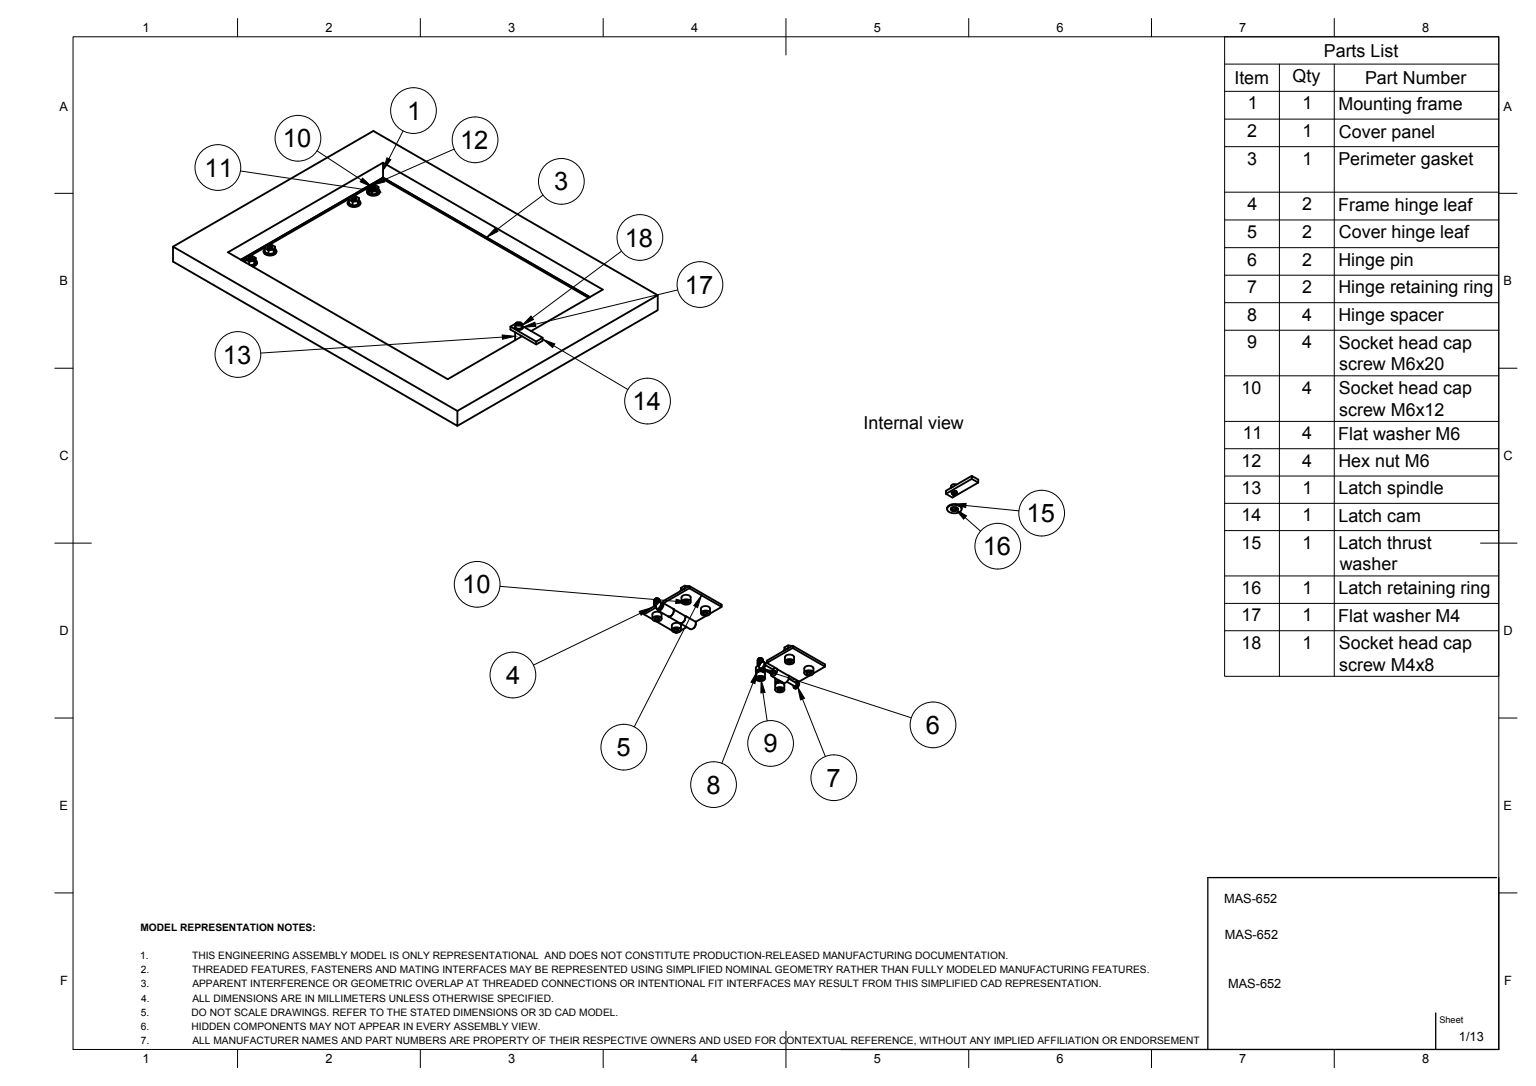
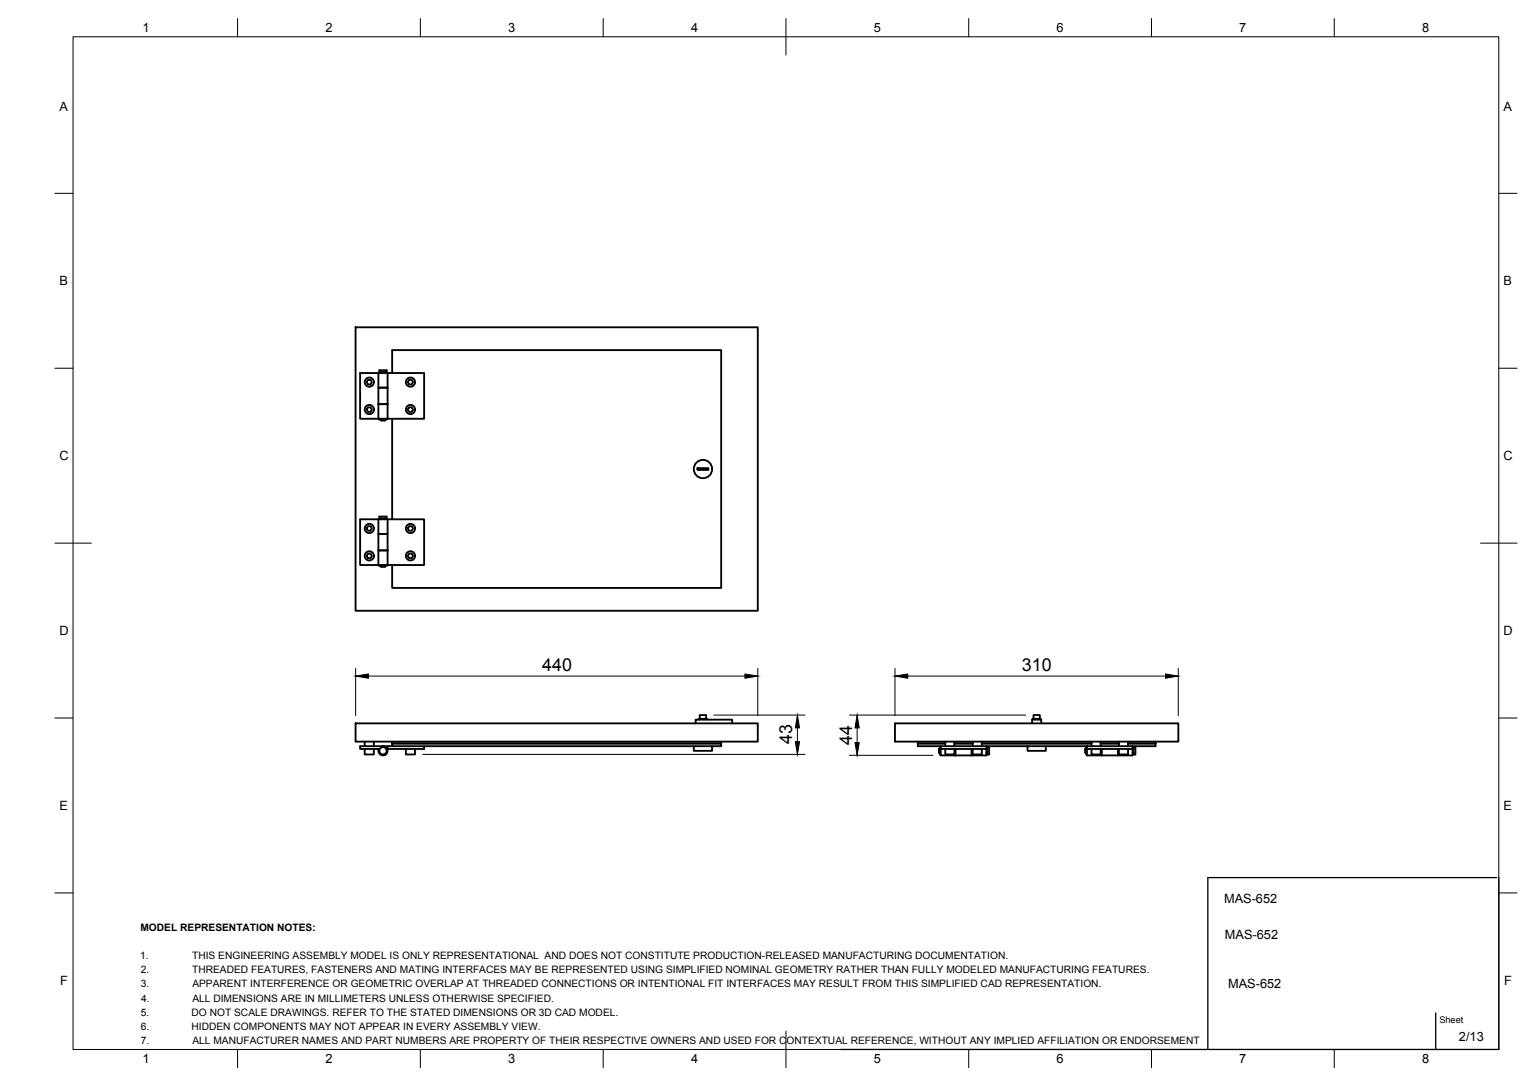
ISO-10303-21;
HEADER;
/* Generated by software containing ST-Developer
 * from STEP Tools, Inc. (www.steptools.com) 
 */

FILE_DESCRIPTION(
/* description */ ('Independent hinged machine back cover with retained hinge pins, perim
eter gasket and quarter-turn cam latch. Nominal cover 360 x 260 x 3 mm
, frame 430 x 300 x 20 mm. No guarding, structural or ingress rating a
ssigned.'),
/* implementation_level */ '2;1');

FILE_NAME(
/* name */ 'MAS-652.step',
/* time_stamp */ '2026-11-09T19:36:59-08:00',
/* author */ (''),
/* organization */ (''),
/* preprocessor_version */ 'ST-DEVELOPER v20.2',
/* originating_system */ 'Autodesk Translation Framework v15.17.0.0',
/* authorisation */ '');

FILE_SCHEMA (('AUTOMOTIVE_DESIGN { 1 0 10303 214 3 1 1 }'));
ENDSEC;

DATA;
#10=MECHANICAL_DESIGN_GEOMETRIC_PRESENTATION_REPRESENTATION('',(#198,#199,
#200,#201,#202,#203,#204,#205,#206,#207,#208,#209,#210,#211,#212,#213,#214,
#215),#32627);
#11=ITEM_DEFINED_TRANSFORMATION($,$,#8893,#9492);
#12=ITEM_DEFINED_TRANSFORMATION($,$,#9080,#9493);
#13=ITEM_DEFINED_TRANSFORMATION($,$,#9102,#9494);
#14=ITEM_DEFINED_TRANSFORMATION($,$,#9267,#9495);
#15=ITEM_DEFINED_TRANSFORMATION($,$,#9323,#9496);
#16=ITEM_DEFINED_TRANSFORMATION($,$,#9294,#9497);
#17=ITEM_DEFINED_TRANSFORMATION($,$,#9312,#9498);
#18=ITEM_DEFINED_TRANSFORMATION($,$,#9345,#9499);
#19=ITEM_DEFINED_TRANSFORMATION($,$,#9354,#9500);
#20=ITEM_DEFINED_TRANSFORMATION($,$,#9414,#9501);
#21=ITEM_DEFINED_TRANSFORMATION($,$,#9458,#9502);
#22=ITEM_DEFINED_TRANSFORMATION($,$,#9467,#9503);
#23=ITEM_DEFINED_TRANSFORMATION($,$,#9113,#9504);
#24=ITEM_DEFINED_TRANSFORMATION($,$,#9183,#9505);
#25=ITEM_DEFINED_TRANSFORMATION($,$,#9196,#9506);
#26=ITEM_DEFINED_TRANSFORMATION($,$,#9205,#9507);
#27=ITEM_DEFINED_TRANSFORMATION($,$,#9216,#9508);
#28=ITEM_DEFINED_TRANSFORMATION($,$,#9225,#9509);
#29=ITEM_DEFINED_TRANSFORMATION($,$,#9267,#9510);
#30=ITEM_DEFINED_TRANSFORMATION($,$,#9294,#9511);
#31=ITEM_DEFINED_TRANSFORMATION($,$,#9312,#9512);
#32=ITEM_DEFINED_TRANSFORMATION($,$,#9323,#9513);
#33=ITEM_DEFINED_TRANSFORMATION($,$,#9345,#9514);
#34=ITEM_DEFINED_TRANSFORMATION($,$,#9354,#9515);
#35=ITEM_DEFINED_TRANSFORMATION($,$,#9414,#9516);
#36=ITEM_DEFINED_TRANSFORMATION($,$,#9458,#9517);
#37=ITEM_DEFINED_TRANSFORMATION($,$,#9467,#9518);
#38=ITEM_DEFINED_TRANSFORMATION($,$,#9345,#9519);
#39=ITEM_DEFINED_TRANSFORMATION($,$,#9354,#9520);
#40=ITEM_DEFINED_TRANSFORMATION($,$,#9414,#9521);
#41=ITEM_DEFINED_TRANSFORMATION($,$,#9458,#9522);
#42=ITEM_DEFINED_TRANSFORMATION($,$,#9467,#9523);
#43=ITEM_DEFINED_TRANSFORMATION($,$,#9345,#9524);
#44=ITEM_DEFINED_TRANSFORMATION($,$,#9354,#9525);
#45=ITEM_DEFINED_TRANSFORMATION($,$,#9414,#9526);
#46=ITEM_DEFINED_TRANSFORMATION($,$,#9458,#9527);
#47=ITEM_DEFINED_TRANSFORMATION($,$,#9467,#9528);
#48=(
REPRESENTATION_RELATIONSHIP($,$,#32708,#32707)
REPRESENTATION_RELATIONSHIP_WITH_TRANSFORMATION(#11)
SHAPE_REPRESENTATION_RELATIONSHIP()
);
#49=(
REPRESENTATION_RELATIONSHIP($,$,#32709,#32707)
REPRESENTATION_RELATIONSHIP_WITH_TRANSFORMATION(#12)
SHAPE_REPRESENTATION_RELATIONSHIP()
);
#50=(
REPRESENTATION_RELATIONSHIP($,$,#32710,#32707)
REPRESENTATION_RELATIONSHIP_WITH_TRANSFORMATION(#13)
SHAPE_REPRESENTATION_RELATIONSHIP()
);
#51=(
REPRESENTATION_RELATIONSHIP($,$,#32717,#32707)
REPRESENTATION_RELATIONSHIP_WITH_TRANSFORMATION(#14)
SHAPE_REPRESENTATION_RELATIONSHIP()
);
#52=(
REPRESENTATION_RELATIONSHIP($,$,#32720,#32707)
REPRESENTATION_RELATIONSHIP_WITH_TRANSFORMATION(#15)
SHAPE_REPRESENTATION_RELATIONSHIP()
);
#53=(
REPRESENTATION_RELATIONSHIP($,$,#32718,#32707)
REPRESENTATION_RELATIONSHIP_WITH_TRANSFORMATION(#16)
SHAPE_REPRESENTATION_RELATIONSHIP()
);
#54=(
REPRESENTATION_RELATIONSHIP($,$,#32719,#32707)
REPRESENTATION_RELATIONSHIP_WITH_TRANSFORMATION(#17)
SHAPE_REPRESENTATION_RELATIONSHIP()
);
#55=(
REPRESENTATION_RELATIONSHIP($,$,#32721,#32707)
REPRESENTATION_RELATIONSHIP_WITH_TRANSFORMATION(#18)
SHAPE_REPRESENTATION_RELATIONSHIP()
);
#56=(
REPRESENTATION_RELATIONSHIP($,$,#32722,#32707)
REPRESENTATION_RELATIONSHIP_WITH_TRANSFORMATION(#19)
SHAPE_REPRESENTATION_RELATIONSHIP()
);
#57=(
REPRESENTATION_RELATIONSHIP($,$,#32723,#32707)
REPRESENTATION_RELATIONSHIP_WITH_TRANSFORMATION(#20)
SHAPE_REPRESENTATION_RELATIONSHIP()
);
#58=(
REPRESENTATION_RELATIONSHIP($,$,#32724,#32707)
REPRESENTATION_RELATIONSHIP_WITH_TRANSFORMATION(#21)
SHAPE_REPRESENTATION_RELATIONSHIP()
);
#59=(
REPRESENTATION_RELATIONSHIP($,$,#32725,#32707)
REPRESENTATION_RELATIONSHIP_WITH_TRANSFORMATION(#22)
SHAPE_REPRESENTATION_RELATIONSHIP()
);
#60=(
REPRESENTATION_RELATIONSHIP($,$,#32711,#32707)
REPRESENTATION_RELATIONSHIP_WITH_TRANSFORMATION(#23)
SHAPE_REPRESENTATION_RELATIONSHIP()
);
#61=(
REPRESENTATION_RELATIONSHIP($,$,#32712,#32707)
REPRESENTATION_RELATIONSHIP_WITH_TRANSFORMATION(#24)
SHAPE_REPRESENTATION_RELATIONSHIP()
);
#62=(
REPRESENTATION_RELATIONSHIP($,$,#32713,#32707)
REPRESENTATION_RELATIONSHIP_WITH_TRANSFORMATION(#25)
SHAPE_REPRESENTATION_RELATIONSHIP()
);
#63=(
REPRESENTATION_RELATIONSHIP($,$,#32714,#32707)
REPRESENTATION_RELATIONSHIP_WITH_TRANSFORMATION(#26)
SHAPE_REPRESENTATION_RELATIONSHIP()
);
#64=(
REPRESENTATION_RELATIONSHIP($,$,#32715,#32707)
REPRESENTATION_RELATIONSHIP_WITH_TRANSFORMATION(#27)
SHAPE_REPRESENTATION_RELATIONSHIP()
);
#65=(
REPRESENTATION_RELATIONSHIP($,$,#32716,#32707)
REPRESENTATION_RELATIONSHIP_WITH_TRANSFORMATION(#28)
SHAPE_REPRESENTATION_RELATIONSHIP()
);
#66=(
REPRESENTATION_RELATIONSHIP($,$,#32717,#32707)
REPRESENTATION_RELATIONSHIP_WITH_TRANSFORMATION(#29)
SHAPE_REPRESENTATION_RELATIONSHIP()
);
#67=(
REPRESENTATION_RELATIONSHIP($,$,#32718,#32707)
REPRESENTATION_RELATIONSHIP_WITH_TRANSFORMATION(#30)
SHAPE_REPRESENTATION_RELATIONSHIP()
);
#68=(
REPRESENTATION_RELATIONSHIP($,$,#32719,#32707)
REPRESENTATION_RELATIONSHIP_WITH_TRANSFORMATION(#31)
SHAPE_REPRESENTATION_RELATIONSHIP()
);
#69=(
REPRESENTATION_RELATIONSHIP($,$,#32720,#32707)
REPRESENTATION_RELATIONSHIP_WITH_TRANSFORMATION(#32)
SHAPE_REPRESENTATION_RELATIONSHIP()
);
#70=(
REPRESENTATION_RELATIONSHIP($,$,#32721,#32707)
REPRESENTATION_RELATIONSHIP_WITH_TRANSFORMATION(#33)
SHAPE_REPRESENTATION_RELATIONSHIP()
);
#71=(
REPRESENTATION_RELATIONSHIP($,$,#32722,#32707)
REPRESENTATION_RELATIONSHIP_WITH_TRANSFORMATION(#34)
SHAPE_REPRESENTATION_RELATIONSHIP()
);
#72=(
REPRESENTATION_RELATIONSHIP($,$,#32723,#32707)
REPRESENTATION_RELATIONSHIP_WITH_TRANSFORMATION(#35)
SHAPE_REPRESENTATION_RELATIONSHIP()
);
#73=(
REPRESENTATION_RELATIONSHIP($,$,#32724,#32707)
REPRESENTATION_RELATIONSHIP_WITH_TRANSFORMATION(#36)
SHAPE_REPRESENTATION_RELATIONSHIP()
);
#74=(
REPRESENTATION_RELATIONSHIP($,$,#32725,#32707)
REPRESENTATION_RELATIONSHIP_WITH_TRANSFORMATION(#37)
SHAPE_REPRESENTATION_RELATIONSHIP()
);
#75=(
REPRESENTATION_RELATIONSHIP($,$,#32721,#32707)
REPRESENTATION_RELATIONSHIP_WITH_TRANSFORMATION(#38)
SHAPE_REPRESENTATION_RELATIONSHIP()
);
#76=(
REPRESENTATION_RELATIONSHIP($,$,#32722,#32707)
REPRESENTATION_RELATIONSHIP_WITH_TRANSFORMATION(#39)
SHAPE_REPRESENTATION_RELATIONSHIP()
);
#77=(
REPRESENTATION_RELATIONSHIP($,$,#32723,#32707)
REPRESENTATION_RELATIONSHIP_WITH_TRANSFORMATION(#40)
SHAPE_REPRESENTATION_RELATIONSHIP()
);
#78=(
REPRESENTATION_RELATIONSHIP($,$,#32724,#32707)
REPRESENTATION_RELATIONSHIP_WITH_TRANSFORMATION(#41)
SHAPE_REPRESENTATION_RELATIONSHIP()
);
#79=(
REPRESENTATION_RELATIONSHIP($,$,#32725,#32707)
REPRESENTATION_RELATIONSHIP_WITH_TRANSFORMATION(#42)
SHAPE_REPRESENTATION_RELATIONSHIP()
);
#80=(
REPRESENTATION_RELATIONSHIP($,$,#32721,#32707)
REPRESENTATION_RELATIONSHIP_WITH_TRANSFORMATION(#43)
SHAPE_REPRESENTATION_RELATIONSHIP()
);
#81=(
REPRESENTATION_RELATIONSHIP($,$,#32722,#32707)
REPRESENTATION_RELATIONSHIP_WITH_TRANSFORMATION(#44)
SHAPE_REPRESENTATION_RELATIONSHIP()
);
#82=(
REPRESENTATION_RELATIONSHIP($,$,#32723,#32707)
REPRESENTATION_RELATIONSHIP_WITH_TRANSFORMATION(#45)
SHAPE_REPRESENTATION_RELATIONSHIP()
);
#83=(
REPRESENTATION_RELATIONSHIP($,$,#32724,#32707)
REPRESENTATION_RELATIONSHIP_WITH_TRANSFORMATION(#46)
SHAPE_REPRESENTATION_RELATIONSHIP()
);
#84=(
REPRESENTATION_RELATIONSHIP($,$,#32725,#32707)
REPRESENTATION_RELATIONSHIP_WITH_TRANSFORMATION(#47)
SHAPE_REPRESENTATION_RELATIONSHIP()
);
#85=CONTEXT_DEPENDENT_SHAPE_REPRESENTATION(#48,#32670);
#86=CONTEXT_DEPENDENT_SHAPE_REPRESENTATION(#49,#32671);
#87=CONTEXT_DEPENDENT_SHAPE_REPRESENTATION(#50,#32672);
#88=CONTEXT_DEPENDENT_SHAPE_REPRESENTATION(#51,#32673);
#89=CONTEXT_DEPENDENT_SHAPE_REPRESENTATION(#52,#32674);
#90=CONTEXT_DEPENDENT_SHAPE_REPRESENTATION(#53,#32675);
#91=CONTEXT_DEPENDENT_SHAPE_REPRESENTATION(#54,#32676);
#92=CONTEXT_DEPENDENT_SHAPE_REPRESENTATION(#55,#32677);
#93=CONTEXT_DEPENDENT_SHAPE_REPRESENTATION(#56,#32678);
#94=CONTEXT_DEPENDENT_SHAPE_REPRESENTATION(#57,#32679);
#95=CONTEXT_DEPENDENT_SHAPE_REPRESENTATION(#58,#32680);
#96=CONTEXT_DEPENDENT_SHAPE_REPRESENTATION(#59,#32681);
#97=CONTEXT_DEPENDENT_SHAPE_REPRESENTATION(#60,#32682);
#98=CONTEXT_DEPENDENT_SHAPE_REPRESENTATION(#61,#32683);
#99=CONTEXT_DEPENDENT_SHAPE_REPRESENTATION(#62,#32684);
#100=CONTEXT_DEPENDENT_SHAPE_REPRESENTATION(#63,#32685);
#101=CONTEXT_DEPENDENT_SHAPE_REPRESENTATION(#64,#32686);
#102=CONTEXT_DEPENDENT_SHAPE_REPRESENTATION(#65,#32687);
#103=CONTEXT_DEPENDENT_SHAPE_REPRESENTATION(#66,#32688);
#104=CONTEXT_DEPENDENT_SHAPE_REPRESENTATION(#67,#32689);
#105=CONTEXT_DEPENDENT_SHAPE_REPRESENTATION(#68,#32690);
#106=CONTEXT_DEPENDENT_SHAPE_REPRESENTATION(#69,#32691);
#107=CONTEXT_DEPENDENT_SHAPE_REPRESENTATION(#70,#32692);
#108=CONTEXT_DEPENDENT_SHAPE_REPRESENTATION(#71,#32693);
#109=CONTEXT_DEPENDENT_SHAPE_REPRESENTATION(#72,#32694);
#110=CONTEXT_DEPENDENT_SHAPE_REPRESENTATION(#73,#32695);
#111=CONTEXT_DEPENDENT_SHAPE_REPRESENTATION(#74,#32696);
#112=CONTEXT_DEPENDENT_SHAPE_REPRESENTATION(#75,#32697);
#113=CONTEXT_DEPENDENT_SHAPE_REPRESENTATION(#76,#32698);
#114=CONTEXT_DEPENDENT_SHAPE_REPRESENTATION(#77,#32699);
#115=CONTEXT_DEPENDENT_SHAPE_REPRESENTATION(#78,#32700);
#116=CONTEXT_DEPENDENT_SHAPE_REPRESENTATION(#79,#32701);
#117=CONTEXT_DEPENDENT_SHAPE_REPRESENTATION(#80,#32702);
#118=CONTEXT_DEPENDENT_SHAPE_REPRESENTATION(#81,#32703);
#119=CONTEXT_DEPENDENT_SHAPE_REPRESENTATION(#82,#32704);
#120=CONTEXT_DEPENDENT_SHAPE_REPRESENTATION(#83,#32705);
#121=CONTEXT_DEPENDENT_SHAPE_REPRESENTATION(#84,#32706);
#122=NEXT_ASSEMBLY_USAGE_OCCURRENCE('Mounting frame:1',
'Mounting frame:1','Mounting frame:1',#32727,#32728,'Mounting frame:1');
#123=NEXT_ASSEMBLY_USAGE_OCCURRENCE('Cover panel:1','Cover panel:1',
'Cover panel:1',#32727,#32729,'Cover panel:1');
#124=NEXT_ASSEMBLY_USAGE_OCCURRENCE('Perimeter gasket:1',
'Perimeter gasket:1','Perimeter gasket:1',#32727,#32730,
'Perimeter gasket:1');
#125=NEXT_ASSEMBLY_USAGE_OCCURRENCE('Frame hinge leaf:1',
'Frame hinge leaf:1','Frame hinge leaf:1',#32727,#32737,
'Frame hinge leaf:1');
#126=NEXT_ASSEMBLY_USAGE_OCCURRENCE('Cover hinge leaf:1',
'Cover hinge leaf:1','Cover hinge leaf:1',#32727,#32740,
'Cover hinge leaf:1');
#127=NEXT_ASSEMBLY_USAGE_OCCURRENCE('Hinge pin:1','Hinge pin:1',
'Hinge pin:1',#32727,#32738,'Hinge pin:1');
#128=NEXT_ASSEMBLY_USAGE_OCCURRENCE('Hinge retaining ring:1',
'Hinge retaining ring:1','Hinge retaining ring:1',#32727,#32739,
'Hinge retaining ring:1');
#129=NEXT_ASSEMBLY_USAGE_OCCURRENCE('Hinge spacer:1','Hinge spacer:1',
'Hinge spacer:1',#32727,#32741,'Hinge spacer:1');
#130=NEXT_ASSEMBLY_USAGE_OCCURRENCE('Socket head cap screw M6x20:1',
'Socket head cap screw M6x20:1','Socket head cap screw M6x20:1',#32727,
#32742,'Socket head cap screw M6x20:1');
#131=NEXT_ASSEMBLY_USAGE_OCCURRENCE('Socket head cap screw M6x12:1',
'Socket head cap screw M6x12:1','Socket head cap screw M6x12:1',#32727,
#32743,'Socket head cap screw M6x12:1');
#132=NEXT_ASSEMBLY_USAGE_OCCURRENCE('Flat washer M6:1',
'Flat washer M6:1','Flat washer M6:1',#32727,#32744,'Flat washer M6:1');
#133=NEXT_ASSEMBLY_USAGE_OCCURRENCE('Hex nut M6:1','Hex nut M6:1',
'Hex nut M6:1',#32727,#32745,'Hex nut M6:1');
#134=NEXT_ASSEMBLY_USAGE_OCCURRENCE('Latch spindle:1','Latch spindle:1',
'Latch spindle:1',#32727,#32731,'Latch spindle:1');
#135=NEXT_ASSEMBLY_USAGE_OCCURRENCE('Latch cam:1','Latch cam:1',
'Latch cam:1',#32727,#32732,'Latch cam:1');
#136=NEXT_ASSEMBLY_USAGE_OCCURRENCE('Latch thrust washer:1',
'Latch thrust washer:1','Latch thrust washer:1',#32727,#32733,
'Latch thrust washer:1');
#137=NEXT_ASSEMBLY_USAGE_OCCURRENCE('Latch retaining ring:1',
'Latch retaining ring:1','Latch retaining ring:1',#32727,#32734,
'Latch retaining ring:1');
#138=NEXT_ASSEMBLY_USAGE_OCCURRENCE('Flat washer M4:1',
'Flat washer M4:1','Flat washer M4:1',#32727,#32735,'Flat washer M4:1');
#139=NEXT_ASSEMBLY_USAGE_OCCURRENCE('Socket head cap screw M4x8:1',
'Socket head cap screw M4x8:1','Socket head cap screw M4x8:1',#32727,#32736,
'Socket head cap screw M4x8:1');
#140=NEXT_ASSEMBLY_USAGE_OCCURRENCE('Frame hinge leaf:2',
'Frame hinge leaf:2','Frame hinge leaf:2',#32727,#32737,
'Frame hinge leaf:2');
#141=NEXT_ASSEMBLY_USAGE_OCCURRENCE('Hinge pin:2','Hinge pin:2',
'Hinge pin:2',#32727,#32738,'Hinge pin:2');
#142=NEXT_ASSEMBLY_USAGE_OCCURRENCE('Hinge retaining ring:2',
'Hinge retaining ring:2','Hinge retaining ring:2',#32727,#32739,
'Hinge retaining ring:2');
#143=NEXT_ASSEMBLY_USAGE_OCCURRENCE('Cover hinge leaf:2',
'Cover hinge leaf:2','Cover hinge leaf:2',#32727,#32740,
'Cover hinge leaf:2');
#144=NEXT_ASSEMBLY_USAGE_OCCURRENCE('Hinge spacer:2','Hinge spacer:2',
'Hinge spacer:2',#32727,#32741,'Hinge spacer:2');
#145=NEXT_ASSEMBLY_USAGE_OCCURRENCE('Socket head cap screw M6x20:2',
'Socket head cap screw M6x20:2','Socket head cap screw M6x20:2',#32727,
#32742,'Socket head cap screw M6x20:2');
#146=NEXT_ASSEMBLY_USAGE_OCCURRENCE('Socket head cap screw M6x12:2',
'Socket head cap screw M6x12:2','Socket head cap screw M6x12:2',#32727,
#32743,'Socket head cap screw M6x12:2');
#147=NEXT_ASSEMBLY_USAGE_OCCURRENCE('Flat washer M6:2',
'Flat washer M6:2','Flat washer M6:2',#32727,#32744,'Flat washer M6:2');
#148=NEXT_ASSEMBLY_USAGE_OCCURRENCE('Hex nut M6:2','Hex nut M6:2',
'Hex nut M6:2',#32727,#32745,'Hex nut M6:2');
#149=NEXT_ASSEMBLY_USAGE_OCCURRENCE('Hinge spacer:3','Hinge spacer:3',
'Hinge spacer:3',#32727,#32741,'Hinge spacer:3');
#150=NEXT_ASSEMBLY_USAGE_OCCURRENCE('Socket head cap screw M6x20:3',
'Socket head cap screw M6x20:3','Socket head cap screw M6x20:3',#32727,
#32742,'Socket head cap screw M6x20:3');
#151=NEXT_ASSEMBLY_USAGE_OCCURRENCE('Socket head cap screw M6x12:3',
'Socket head cap screw M6x12:3','Socket head cap screw M6x12:3',#32727,
#32743,'Socket head cap screw M6x12:3');
#152=NEXT_ASSEMBLY_USAGE_OCCURRENCE('Flat washer M6:3',
'Flat washer M6:3','Flat washer M6:3',#32727,#32744,'Flat washer M6:3');
#153=NEXT_ASSEMBLY_USAGE_OCCURRENCE('Hex nut M6:3','Hex nut M6:3',
'Hex nut M6:3',#32727,#32745,'Hex nut M6:3');
#154=NEXT_ASSEMBLY_USAGE_OCCURRENCE('Hinge spacer:4','Hinge spacer:4',
'Hinge spacer:4',#32727,#32741,'Hinge spacer:4');
#155=NEXT_ASSEMBLY_USAGE_OCCURRENCE('Socket head cap screw M6x20:4',
'Socket head cap screw M6x20:4','Socket head cap screw M6x20:4',#32727,
#32742,'Socket head cap screw M6x20:4');
#156=NEXT_ASSEMBLY_USAGE_OCCURRENCE('Socket head cap screw M6x12:4',
'Socket head cap screw M6x12:4','Socket head cap screw M6x12:4',#32727,
#32743,'Socket head cap screw M6x12:4');
#157=NEXT_ASSEMBLY_USAGE_OCCURRENCE('Flat washer M6:4',
'Flat washer M6:4','Flat washer M6:4',#32727,#32744,'Flat washer M6:4');
#158=NEXT_ASSEMBLY_USAGE_OCCURRENCE('Hex nut M6:4','Hex nut M6:4',
'Hex nut M6:4',#32727,#32745,'Hex nut M6:4');
#159=CONICAL_SURFACE('',#9248,1.5,0.785398163397448);
#160=CONICAL_SURFACE('',#9395,2.5,0.785398163397448);
#161=CONICAL_SURFACE('',#9439,2.5,0.785398163397449);
#162=SHAPE_REPRESENTATION_RELATIONSHIP('SRR','None',#32708,#180);
#163=SHAPE_REPRESENTATION_RELATIONSHIP('SRR','None',#32709,#181);
#164=SHAPE_REPRESENTATION_RELATIONSHIP('SRR','None',#32710,#182);
#165=SHAPE_REPRESENTATION_RELATIONSHIP('SRR','None',#32711,#183);
#166=SHAPE_REPRESENTATION_RELATIONSHIP('SRR','None',#32712,#184);
#167=SHAPE_REPRESENTATION_RELATIONSHIP('SRR','None',#32713,#185);
#168=SHAPE_REPRESENTATION_RELATIONSHIP('SRR','None',#32714,#186);
#169=SHAPE_REPRESENTATION_RELATIONSHIP('SRR','None',#32715,#187);
#170=SHAPE_REPRESENTATION_RELATIONSHIP('SRR','None',#32716,#188);
#171=SHAPE_REPRESENTATION_RELATIONSHIP('SRR','None',#32717,#189);
#172=SHAPE_REPRESENTATION_RELATIONSHIP('SRR','None',#32718,#190);
#173=SHAPE_REPRESENTATION_RELATIONSHIP('SRR','None',#32719,#191);
#174=SHAPE_REPRESENTATION_RELATIONSHIP('SRR','None',#32720,#192);
#175=SHAPE_REPRESENTATION_RELATIONSHIP('SRR','None',#32721,#193);
#176=SHAPE_REPRESENTATION_RELATIONSHIP('SRR','None',#32722,#194);
#177=SHAPE_REPRESENTATION_RELATIONSHIP('SRR','None',#32723,#195);
#178=SHAPE_REPRESENTATION_RELATIONSHIP('SRR','None',#32724,#196);
#179=SHAPE_REPRESENTATION_RELATIONSHIP('SRR','None',#32725,#197);
#180=ADVANCED_BREP_SHAPE_REPRESENTATION('',(#216),#32609);
#181=ADVANCED_BREP_SHAPE_REPRESENTATION('',(#217),#32610);
#182=ADVANCED_BREP_SHAPE_REPRESENTATION('',(#218),#32611);
#183=ADVANCED_BREP_SHAPE_REPRESENTATION('',(#219),#32612);
#184=ADVANCED_BREP_SHAPE_REPRESENTATION('',(#220),#32613);
#185=ADVANCED_BREP_SHAPE_REPRESENTATION('',(#221),#32614);
#186=ADVANCED_BREP_SHAPE_REPRESENTATION('',(#222),#32615);
#187=ADVANCED_BREP_SHAPE_REPRESENTATION('',(#223),#32616);
#188=ADVANCED_BREP_SHAPE_REPRESENTATION('',(#224),#32617);
#189=ADVANCED_BREP_SHAPE_REPRESENTATION('',(#225),#32618);
#190=ADVANCED_BREP_SHAPE_REPRESENTATION('',(#226),#32619);
#191=ADVANCED_BREP_SHAPE_REPRESENTATION('',(#227),#32620);
#192=ADVANCED_BREP_SHAPE_REPRESENTATION('',(#228),#32621);
#193=ADVANCED_BREP_SHAPE_REPRESENTATION('',(#229),#32622);
#194=ADVANCED_BREP_SHAPE_REPRESENTATION('',(#230),#32623);
#195=ADVANCED_BREP_SHAPE_REPRESENTATION('',(#231),#32624);
#196=ADVANCED_BREP_SHAPE_REPRESENTATION('',(#232),#32625);
#197=ADVANCED_BREP_SHAPE_REPRESENTATION('',(#233),#32626);
#198=STYLED_ITEM('',(#32807),#216);
#199=STYLED_ITEM('',(#32808),#217);
#200=STYLED_ITEM('',(#32809),#218);
#201=STYLED_ITEM('',(#32810),#219);
#202=STYLED_ITEM('',(#32811),#220);
#203=STYLED_ITEM('',(#32812),#221);
#204=STYLED_ITEM('',(#32809),#222);
#205=STYLED_ITEM('',(#32812),#223);
#206=STYLED_ITEM('',(#32809),#224);
#207=STYLED_ITEM('',(#32810),#225);
#208=STYLED_ITEM('',(#32812),#226);
#209=STYLED_ITEM('',(#32809),#227);
#210=STYLED_ITEM('',(#32811),#228);
#211=STYLED_ITEM('',(#32812),#229);
#212=STYLED_ITEM('',(#32809),#230);
#213=STYLED_ITEM('',(#32809),#231);
#214=STYLED_ITEM('',(#32812),#232);
#215=STYLED_ITEM('',(#32810),#233);
#216=MANIFOLD_SOLID_BREP('Body1',#8675);
#217=MANIFOLD_SOLID_BREP('Body1',#8676);
#218=MANIFOLD_SOLID_BREP('Body1',#8677);
#219=MANIFOLD_SOLID_BREP('Body1',#8678);
#220=MANIFOLD_SOLID_BREP('Body1',#8679);
#221=MANIFOLD_SOLID_BREP('Body1',#8680);
#222=MANIFOLD_SOLID_BREP('Body1',#8681);
#223=MANIFOLD_SOLID_BREP('Body1',#8682);
#224=MANIFOLD_SOLID_BREP('Body1',#8683);
#225=MANIFOLD_SOLID_BREP('Body1',#8684);
#226=MANIFOLD_SOLID_BREP('Body1',#8685);
#227=MANIFOLD_SOLID_BREP('Body1',#8686);
#228=MANIFOLD_SOLID_BREP('Body1',#8687);
#229=MANIFOLD_SOLID_BREP('Body1',#8688);
#230=MANIFOLD_SOLID_BREP('Body1',#8689);
#231=MANIFOLD_SOLID_BREP('Body1',#8690);
#232=MANIFOLD_SOLID_BREP('Body1',#8691);
#233=MANIFOLD_SOLID_BREP('Body1',#8692);
#234=FACE_BOUND('',#1096,.T.);
#235=FACE_BOUND('',#1098,.T.);
#236=FACE_BOUND('',#1099,.T.);
#237=FACE_BOUND('',#1100,.T.);
#238=FACE_BOUND('',#1101,.T.);
#239=FACE_BOUND('',#1102,.T.);
#240=FACE_BOUND('',#1113,.T.);
#241=FACE_BOUND('',#1114,.T.);
#242=FACE_BOUND('',#1115,.T.);
#243=FACE_BOUND('',#1116,.T.);
#244=FACE_BOUND('',#1117,.T.);
#245=FACE_BOUND('',#1119,.T.);
#246=FACE_BOUND('',#1120,.T.);
#247=FACE_BOUND('',#1121,.T.);
#248=FACE_BOUND('',#1122,.T.);
#249=FACE_BOUND('',#1123,.T.);
#250=FACE_BOUND('',#1133,.T.);
#251=FACE_BOUND('',#1135,.T.);
#252=FACE_BOUND('',#1180,.T.);
#253=FACE_BOUND('',#1182,.T.);
#254=FACE_BOUND('',#1191,.T.);
#255=FACE_BOUND('',#1193,.T.);
#256=FACE_BOUND('',#1196,.T.);
#257=FACE_BOUND('',#1199,.T.);
#258=FACE_BOUND('',#1211,.T.);
#259=FACE_BOUND('',#1213,.T.);
#260=FACE_BOUND('',#1217,.T.);
#261=FACE_BOUND('',#1219,.T.);
#262=FACE_BOUND('',#1229,.T.);
#263=FACE_BOUND('',#1231,.T.);
#264=FACE_BOUND('',#1265,.T.);
#265=FACE_BOUND('',#1268,.T.);
#266=FACE_BOUND('',#1272,.T.);
#267=FACE_BOUND('',#1273,.T.);
#268=FACE_BOUND('',#1279,.T.);
#269=FACE_BOUND('',#1281,.T.);
#270=FACE_BOUND('',#1285,.T.);
#271=FACE_BOUND('',#1287,.T.);
#272=FACE_BOUND('',#1290,.T.);
#273=FACE_BOUND('',#1291,.T.);
#274=FACE_BOUND('',#1294,.T.);
#275=FACE_BOUND('',#1296,.T.);
#276=FACE_BOUND('',#1299,.T.);
#277=FACE_BOUND('',#1313,.T.);
#278=FACE_BOUND('',#1314,.T.);
#279=FACE_BOUND('',#1319,.T.);
#280=FACE_BOUND('',#1323,.T.);
#281=FACE_BOUND('',#1327,.T.);
#282=FACE_BOUND('',#1328,.T.);
#283=FACE_BOUND('',#1332,.T.);
#284=FACE_BOUND('',#1334,.T.);
#285=FACE_BOUND('',#1386,.T.);
#286=FACE_BOUND('',#1389,.T.);
#287=FACE_BOUND('',#1426,.T.);
#288=FACE_BOUND('',#1429,.T.);
#289=FACE_BOUND('',#1434,.T.);
#290=FACE_BOUND('',#1436,.T.);
#291=FACE_BOUND('',#1451,.T.);
#292=FACE_BOUND('',#1460,.T.);
#293=B_SPLINE_SURFACE_WITH_KNOTS('',3,3,((#16428,#16429,#16430,#16431,#16432,
#16433,#16434,#16435,#16436,#16437,#16438,#16439,#16440,#16441,#16442,#16443,
#16444,#16445,#16446,#16447,#16448,#16449,#16450,#16451,#16452,#16453,#16454,
#16455,#16456,#16457,#16458,#16459,#16460,#16461,#16462,#16463,#16464,#16465,
#16466,#16467,#16468,#16469,#16470,#16471,#16472,#16473,#16474,#16475,#16476,
#16477,#16478,#16479,#16480,#16481,#16482,#16483,#16484,#16485,#16486,#16487,
#16488,#16489,#16490,#16491,#16492,#16493,#16494,#16495,#16496,#16497,#16498,
#16499,#16500,#16501,#16502,#16503,#16504,#16505,#16506,#16507,#16508,#16509,
#16510,#16511,#16512,#16513,#16514,#16515,#16516,#16517,#16518,#16519,#16520,
#16521,#16522,#16523,#16524,#16525,#16526,#16527,#16528,#16529,#16530,#16531,
#16532,#16533,#16534,#16535,#16536,#16537,#16538,#16539),(#16540,#16541,
#16542,#16543,#16544,#16545,#16546,#16547,#16548,#16549,#16550,#16551,#16552,
#16553,#16554,#16555,#16556,#16557,#16558,#16559,#16560,#16561,#16562,#16563,
#16564,#16565,#16566,#16567,#16568,#16569,#16570,#16571,#16572,#16573,#16574,
#16575,#16576,#16577,#16578,#16579,#16580,#16581,#16582,#16583,#16584,#16585,
#16586,#16587,#16588,#16589,#16590,#16591,#16592,#16593,#16594,#16595,#16596,
#16597,#16598,#16599,#16600,#16601,#16602,#16603,#16604,#16605,#16606,#16607,
#16608,#16609,#16610,#16611,#16612,#16613,#16614,#16615,#16616,#16617,#16618,
#16619,#16620,#16621,#16622,#16623,#16624,#16625,#16626,#16627,#16628,#16629,
#16630,#16631,#16632,#16633,#16634,#16635,#16636,#16637,#16638,#16639,#16640,
#16641,#16642,#16643,#16644,#16645,#16646,#16647,#16648,#16649,#16650,#16651),
(#16652,#16653,#16654,#16655,#16656,#16657,#16658,#16659,#16660,#16661,
#16662,#16663,#16664,#16665,#16666,#16667,#16668,#16669,#16670,#16671,#16672,
#16673,#16674,#16675,#16676,#16677,#16678,#16679,#16680,#16681,#16682,#16683,
#16684,#16685,#16686,#16687,#16688,#16689,#16690,#16691,#16692,#16693,#16694,
#16695,#16696,#16697,#16698,#16699,#16700,#16701,#16702,#16703,#16704,#16705,
#16706,#16707,#16708,#16709,#16710,#16711,#16712,#16713,#16714,#16715,#16716,
#16717,#16718,#16719,#16720,#16721,#16722,#16723,#16724,#16725,#16726,#16727,
#16728,#16729,#16730,#16731,#16732,#16733,#16734,#16735,#16736,#16737,#16738,
#16739,#16740,#16741,#16742,#16743,#16744,#16745,#16746,#16747,#16748,#16749,
#16750,#16751,#16752,#16753,#16754,#16755,#16756,#16757,#16758,#16759,#16760,
#16761,#16762,#16763),(#16764,#16765,#16766,#16767,#16768,#16769,#16770,
#16771,#16772,#16773,#16774,#16775,#16776,#16777,#16778,#16779,#16780,#16781,
#16782,#16783,#16784,#16785,#16786,#16787,#16788,#16789,#16790,#16791,#16792,
#16793,#16794,#16795,#16796,#16797,#16798,#16799,#16800,#16801,#16802,#16803,
#16804,#16805,#16806,#16807,#16808,#16809,#16810,#16811,#16812,#16813,#16814,
#16815,#16816,#16817,#16818,#16819,#16820,#16821,#16822,#16823,#16824,#16825,
#16826,#16827,#16828,#16829,#16830,#16831,#16832,#16833,#16834,#16835,#16836,
#16837,#16838,#16839,#16840,#16841,#16842,#16843,#16844,#16845,#16846,#16847,
#16848,#16849,#16850,#16851,#16852,#16853,#16854,#16855,#16856,#16857,#16858,
#16859,#16860,#16861,#16862,#16863,#16864,#16865,#16866,#16867,#16868,#16869,
#16870,#16871,#16872,#16873,#16874,#16875)),.UNSPECIFIED.,.F.,.F.,.F.,(4,
4),(4,1,1,1,1,1,1,1,1,1,1,1,1,1,1,1,1,1,1,1,1,1,1,1,1,1,1,1,1,1,1,1,1,1,
1,1,1,1,1,1,1,1,1,1,1,1,1,1,1,1,1,1,1,1,1,1,1,1,1,1,1,1,1,1,1,1,1,1,1,1,
1,1,1,1,1,1,1,1,1,1,1,1,1,1,1,1,1,1,1,1,1,1,1,1,1,1,1,1,1,1,1,1,1,1,1,1,
1,1,1,4),(0.,0.064201349933888),(11.8589888623077,12.8574392762075,13.8558896901074,
14.8543401040072,15.852790517907,16.8512409318069,17.8496913457067,18.8481417596065,
19.8465921735064,20.8450425874062,21.843493001306,22.8419434152058,23.8403938291057,
24.8388442430055,25.8372946569053,26.8357450708052,27.834195484705,28.8326458986048,
29.8310963125046,30.8295467264045,31.8279971403043,32.8264475542041,33.824897968104,
34.8233483820038,35.8217987959036,36.8202492098035,37.8186996237033,38.8171500376031,
39.8156004515029,40.8140508654028,41.8125012793026,42.8109516932024,43.8094021071023,
44.8078525210021,45.8063029349019,46.8047533488018,47.8032037627016,48.8016541766014,
49.8001045905012,50.7985550044011,51.7970054183009,52.7954558322007,53.7939062461006,
54.7923566600004,55.7908070739002,56.7892574878001,57.7877079016999,58.7861583155997,
59.7846087294995,60.7830591433994,61.7815095572992,62.779959971199,63.7784103850989,
64.7768607989987,65.7753112128985,66.7737616267983,67.7722120406982,68.770662454598,
69.7691128684978,70.7675632823977,71.7660136962975,72.7644641101973,73.7629145240972,
74.761364937997,75.7598153518968,76.7582657657966,77.7567161796965,78.7551665935963,
79.7536170074961,80.7520674213959,81.7505178352958,82.7489682491956,83.7474186630954,
84.7458690769953,85.7443194908951,86.7427699047949,87.7412203186948,88.7396707325946,
89.7381211464944,90.7365715603943,91.7350219742941,92.7334723881939,93.7319228020937,
94.7303732159936,95.7288236298934,96.7272740437932,97.7257244576931,98.7241748715929,
99.7226252854927,100.721075699393,101.719526113292,102.717976527192,103.716426941092,
104.714877354992,105.713327768892,106.711778182792,107.710228596691,108.708679010591,
109.707129424491,110.705579838391,111.704030252291,112.70248066619,113.70093108009,
114.69938149399,115.69783190789,116.69628232179,117.69473273569,118.693183149589,
119.691633563489,120.690083977389),.UNSPECIFIED.);
#294=B_SPLINE_SURFACE_WITH_KNOTS('',3,3,((#16998,#16999,#17000,#17001,#17002,
#17003,#17004,#17005,#17006,#17007,#17008,#17009,#17010,#17011,#17012,#17013,
#17014,#17015,#17016,#17017,#17018,#17019,#17020,#17021,#17022,#17023,#17024,
#17025,#17026,#17027,#17028,#17029,#17030,#17031,#17032,#17033,#17034,#17035,
#17036,#17037,#17038,#17039,#17040,#17041,#17042,#17043,#17044,#17045,#17046,
#17047,#17048,#17049,#17050,#17051,#17052,#17053,#17054,#17055,#17056,#17057,
#17058,#17059,#17060,#17061,#17062,#17063,#17064,#17065,#17066,#17067,#17068,
#17069,#17070,#17071,#17072,#17073,#17074,#17075,#17076,#17077,#17078,#17079,
#17080,#17081,#17082,#17083,#17084,#17085,#17086,#17087,#17088,#17089,#17090,
#17091,#17092,#17093,#17094,#17095,#17096,#17097,#17098,#17099,#17100,#17101,
#17102,#17103,#17104,#17105,#17106,#17107,#17108,#17109),(#17110,#17111,
#17112,#17113,#17114,#17115,#17116,#17117,#17118,#17119,#17120,#17121,#17122,
#17123,#17124,#17125,#17126,#17127,#17128,#17129,#17130,#17131,#17132,#17133,
#17134,#17135,#17136,#17137,#17138,#17139,#17140,#17141,#17142,#17143,#17144,
#17145,#17146,#17147,#17148,#17149,#17150,#17151,#17152,#17153,#17154,#17155,
#17156,#17157,#17158,#17159,#17160,#17161,#17162,#17163,#17164,#17165,#17166,
#17167,#17168,#17169,#17170,#17171,#17172,#17173,#17174,#17175,#17176,#17177,
#17178,#17179,#17180,#17181,#17182,#17183,#17184,#17185,#17186,#17187,#17188,
#17189,#17190,#17191,#17192,#17193,#17194,#17195,#17196,#17197,#17198,#17199,
#17200,#17201,#17202,#17203,#17204,#17205,#17206,#17207,#17208,#17209,#17210,
#17211,#17212,#17213,#17214,#17215,#17216,#17217,#17218,#17219,#17220,#17221),
(#17222,#17223,#17224,#17225,#17226,#17227,#17228,#17229,#17230,#17231,
#17232,#17233,#17234,#17235,#17236,#17237,#17238,#17239,#17240,#17241,#17242,
#17243,#17244,#17245,#17246,#17247,#17248,#17249,#17250,#17251,#17252,#17253,
#17254,#17255,#17256,#17257,#17258,#17259,#17260,#17261,#17262,#17263,#17264,
#17265,#17266,#17267,#17268,#17269,#17270,#17271,#17272,#17273,#17274,#17275,
#17276,#17277,#17278,#17279,#17280,#17281,#17282,#17283,#17284,#17285,#17286,
#17287,#17288,#17289,#17290,#17291,#17292,#17293,#17294,#17295,#17296,#17297,
#17298,#17299,#17300,#17301,#17302,#17303,#17304,#17305,#17306,#17307,#17308,
#17309,#17310,#17311,#17312,#17313,#17314,#17315,#17316,#17317,#17318,#17319,
#17320,#17321,#17322,#17323,#17324,#17325,#17326,#17327,#17328,#17329,#17330,
#17331,#17332,#17333),(#17334,#17335,#17336,#17337,#17338,#17339,#17340,
#17341,#17342,#17343,#17344,#17345,#17346,#17347,#17348,#17349,#17350,#17351,
#17352,#17353,#17354,#17355,#17356,#17357,#17358,#17359,#17360,#17361,#17362,
#17363,#17364,#17365,#17366,#17367,#17368,#17369,#17370,#17371,#17372,#17373,
#17374,#17375,#17376,#17377,#17378,#17379,#17380,#17381,#17382,#17383,#17384,
#17385,#17386,#17387,#17388,#17389,#17390,#17391,#17392,#17393,#17394,#17395,
#17396,#17397,#17398,#17399,#17400,#17401,#17402,#17403,#17404,#17405,#17406,
#17407,#17408,#17409,#17410,#17411,#17412,#17413,#17414,#17415,#17416,#17417,
#17418,#17419,#17420,#17421,#17422,#17423,#17424,#17425,#17426,#17427,#17428,
#17429,#17430,#17431,#17432,#17433,#17434,#17435,#17436,#17437,#17438,#17439,
#17440,#17441,#17442,#17443,#17444,#17445)),.UNSPECIFIED.,.F.,.F.,.F.,(4,
4),(4,1,1,1,1,1,1,1,1,1,1,1,1,1,1,1,1,1,1,1,1,1,1,1,1,1,1,1,1,1,1,1,1,1,
1,1,1,1,1,1,1,1,1,1,1,1,1,1,1,1,1,1,1,1,1,1,1,1,1,1,1,1,1,1,1,1,1,1,1,1,
1,1,1,1,1,1,1,1,1,1,1,1,1,1,1,1,1,1,1,1,1,1,1,1,1,1,1,1,1,1,1,1,1,1,1,1,
1,1,1,4),(0.,0.064201349933888),(14.3984001269718,15.3968505408716,16.3953009547714,
17.3937513686712,18.3922017825711,19.3906521964709,20.3891026103707,21.3875530242706,
22.3860034381704,23.3844538520702,24.3829042659701,25.3813546798699,26.3798050937697,
27.3782555076695,28.3767059215694,29.3751563354692,30.373606749369,31.3720571632689,
32.3705075771687,33.3689579910685,34.3674084049683,35.3658588188682,36.364309232768,
37.3627596466678,38.3612100605677,39.3596604744675,40.3581108883673,41.3565613022672,
42.355011716167,43.3534621300668,44.3519125439666,45.3503629578665,46.3488133717663,
47.3472637856661,48.345714199566,49.3441646134658,50.3426150273656,51.3410654412654,
52.3395158551653,53.3379662690651,54.3364166829649,55.3348670968648,56.3333175107646,
57.3317679246644,58.3302183385643,59.3286687524641,60.3271191663639,61.3255695802637,
62.3240199941636,63.3224704080634,64.3209208219632,65.3193712358631,66.3178216497629,
67.3162720636627,68.3147224775625,69.3131728914624,70.3116233053622,71.310073719262,
72.3085241331619,73.3069745470617,74.3054249609615,75.3038753748613,76.3023257887612,
77.300776202661,78.2992266165608,79.2976770304607,80.2961274443605,81.2945778582603,
82.2930282721602,83.29147868606,84.2899290999598,85.2883795138596,86.2868299277595,
87.2852803416593,88.2837307555591,89.282181169459,90.2806315833588,91.2790819972586,
92.2775324111584,93.2759828250583,94.2744332389581,95.2728836528579,96.2713340667578,
97.2697844806576,98.2682348945574,99.2666853084573,100.265135722357,101.263586136257,
102.262036550157,103.260486964057,104.258937377956,105.257387791856,106.255838205756,
107.254288619656,108.252739033556,109.251189447456,110.249639861355,111.248090275255,
112.246540689155,113.244991103055,114.243441516955,115.241891930855,116.240342344754,
117.238792758654,118.237243172554,119.235693586454,120.234144000354,121.232594414253,
122.231044828153,123.229495242053),.UNSPECIFIED.);
#295=B_SPLINE_SURFACE_WITH_KNOTS('',3,3,((#17768,#17769,#17770,#17771,#17772,
#17773,#17774,#17775,#17776,#17777,#17778,#17779,#17780,#17781,#17782,#17783,
#17784,#17785,#17786,#17787,#17788,#17789,#17790,#17791,#17792,#17793,#17794,
#17795,#17796,#17797,#17798,#17799,#17800,#17801,#17802,#17803,#17804,#17805,
#17806,#17807,#17808,#17809,#17810,#17811,#17812,#17813,#17814,#17815,#17816,
#17817,#17818,#17819,#17820,#17821,#17822,#17823,#17824,#17825,#17826,#17827,
#17828,#17829,#17830,#17831,#17832,#17833,#17834,#17835,#17836,#17837,#17838,
#17839,#17840,#17841,#17842,#17843,#17844,#17845,#17846,#17847,#17848,#17849,
#17850,#17851,#17852,#17853,#17854,#17855,#17856,#17857,#17858,#17859,#17860,
#17861,#17862,#17863,#17864,#17865,#17866,#17867,#17868,#17869,#17870,#17871,
#17872,#17873,#17874,#17875,#17876,#17877,#17878,#17879),(#17880,#17881,
#17882,#17883,#17884,#17885,#17886,#17887,#17888,#17889,#17890,#17891,#17892,
#17893,#17894,#17895,#17896,#17897,#17898,#17899,#17900,#17901,#17902,#17903,
#17904,#17905,#17906,#17907,#17908,#17909,#17910,#17911,#17912,#17913,#17914,
#17915,#17916,#17917,#17918,#17919,#17920,#17921,#17922,#17923,#17924,#17925,
#17926,#17927,#17928,#17929,#17930,#17931,#17932,#17933,#17934,#17935,#17936,
#17937,#17938,#17939,#17940,#17941,#17942,#17943,#17944,#17945,#17946,#17947,
#17948,#17949,#17950,#17951,#17952,#17953,#17954,#17955,#17956,#17957,#17958,
#17959,#17960,#17961,#17962,#17963,#17964,#17965,#17966,#17967,#17968,#17969,
#17970,#17971,#17972,#17973,#17974,#17975,#17976,#17977,#17978,#17979,#17980,
#17981,#17982,#17983,#17984,#17985,#17986,#17987,#17988,#17989,#17990,#17991),
(#17992,#17993,#17994,#17995,#17996,#17997,#17998,#17999,#18000,#18001,
#18002,#18003,#18004,#18005,#18006,#18007,#18008,#18009,#18010,#18011,#18012,
#18013,#18014,#18015,#18016,#18017,#18018,#18019,#18020,#18021,#18022,#18023,
#18024,#18025,#18026,#18027,#18028,#18029,#18030,#18031,#18032,#18033,#18034,
#18035,#18036,#18037,#18038,#18039,#18040,#18041,#18042,#18043,#18044,#18045,
#18046,#18047,#18048,#18049,#18050,#18051,#18052,#18053,#18054,#18055,#18056,
#18057,#18058,#18059,#18060,#18061,#18062,#18063,#18064,#18065,#18066,#18067,
#18068,#18069,#18070,#18071,#18072,#18073,#18074,#18075,#18076,#18077,#18078,
#18079,#18080,#18081,#18082,#18083,#18084,#18085,#18086,#18087,#18088,#18089,
#18090,#18091,#18092,#18093,#18094,#18095,#18096,#18097,#18098,#18099,#18100,
#18101,#18102,#18103),(#18104,#18105,#18106,#18107,#18108,#18109,#18110,
#18111,#18112,#18113,#18114,#18115,#18116,#18117,#18118,#18119,#18120,#18121,
#18122,#18123,#18124,#18125,#18126,#18127,#18128,#18129,#18130,#18131,#18132,
#18133,#18134,#18135,#18136,#18137,#18138,#18139,#18140,#18141,#18142,#18143,
#18144,#18145,#18146,#18147,#18148,#18149,#18150,#18151,#18152,#18153,#18154,
#18155,#18156,#18157,#18158,#18159,#18160,#18161,#18162,#18163,#18164,#18165,
#18166,#18167,#18168,#18169,#18170,#18171,#18172,#18173,#18174,#18175,#18176,
#18177,#18178,#18179,#18180,#18181,#18182,#18183,#18184,#18185,#18186,#18187,
#18188,#18189,#18190,#18191,#18192,#18193,#18194,#18195,#18196,#18197,#18198,
#18199,#18200,#18201,#18202,#18203,#18204,#18205,#18206,#18207,#18208,#18209,
#18210,#18211,#18212,#18213,#18214,#18215)),.UNSPECIFIED.,.F.,.F.,.F.,(4,
4),(4,1,1,1,1,1,1,1,1,1,1,1,1,1,1,1,1,1,1,1,1,1,1,1,1,1,1,1,1,1,1,1,1,1,
1,1,1,1,1,1,1,1,1,1,1,1,1,1,1,1,1,1,1,1,1,1,1,1,1,1,1,1,1,1,1,1,1,1,1,1,
1,1,1,1,1,1,1,1,1,1,1,1,1,1,1,1,1,1,1,1,1,1,1,1,1,1,1,1,1,1,1,1,1,1,1,1,
1,1,1,4),(0.,0.064201349933888),(11.8589888623077,12.8574392762076,13.8558896901074,
14.8543401040072,15.852790517907,16.8512409318069,17.8496913457067,18.8481417596065,
19.8465921735064,20.8450425874062,21.843493001306,22.8419434152058,23.8403938291057,
24.8388442430055,25.8372946569053,26.8357450708052,27.834195484705,28.8326458986048,
29.8310963125047,30.8295467264045,31.8279971403043,32.8264475542041,33.824897968104,
34.8233483820038,35.8217987959036,36.8202492098035,37.8186996237033,38.8171500376031,
39.8156004515029,40.8140508654028,41.8125012793026,42.8109516932024,43.8094021071023,
44.8078525210021,45.8063029349019,46.8047533488018,47.8032037627016,48.8016541766014,
49.8001045905012,50.7985550044011,51.7970054183009,52.7954558322007,53.7939062461006,
54.7923566600004,55.7908070739002,56.7892574878001,57.7877079016999,58.7861583155997,
59.7846087294995,60.7830591433994,61.7815095572992,62.779959971199,63.7784103850989,
64.7768607989987,65.7753112128985,66.7737616267983,67.7722120406982,68.770662454598,
69.7691128684978,70.7675632823977,71.7660136962975,72.7644641101973,73.7629145240971,
74.761364937997,75.7598153518968,76.7582657657966,77.7567161796965,78.7551665935963,
79.7536170074961,80.7520674213959,81.7505178352958,82.7489682491956,83.7474186630954,
84.7458690769953,85.7443194908951,86.7427699047949,87.7412203186948,88.7396707325946,
89.7381211464944,90.7365715603942,91.7350219742941,92.7334723881939,93.7319228020937,
94.7303732159936,95.7288236298934,96.7272740437932,97.725724457693,98.7241748715929,
99.7226252854927,100.721075699393,101.719526113292,102.717976527192,103.716426941092,
104.714877354992,105.713327768892,106.711778182792,107.710228596691,108.708679010591,
109.707129424491,110.705579838391,111.704030252291,112.70248066619,113.70093108009,
114.69938149399,115.69783190789,116.69628232179,117.69473273569,118.693183149589,
119.691633563489,120.690083977389),.UNSPECIFIED.);
#296=B_SPLINE_SURFACE_WITH_KNOTS('',3,3,((#18338,#18339,#18340,#18341,#18342,
#18343,#18344,#18345,#18346,#18347,#18348,#18349,#18350,#18351,#18352,#18353,
#18354,#18355,#18356,#18357,#18358,#18359,#18360,#18361,#18362,#18363,#18364,
#18365,#18366,#18367,#18368,#18369,#18370,#18371,#18372,#18373,#18374,#18375,
#18376,#18377,#18378,#18379,#18380,#18381,#18382,#18383,#18384,#18385,#18386,
#18387,#18388,#18389,#18390,#18391,#18392,#18393,#18394,#18395,#18396,#18397,
#18398,#18399,#18400,#18401,#18402,#18403,#18404,#18405,#18406,#18407,#18408,
#18409,#18410,#18411,#18412,#18413,#18414,#18415,#18416,#18417,#18418,#18419,
#18420,#18421,#18422,#18423,#18424,#18425,#18426,#18427,#18428,#18429,#18430,
#18431,#18432,#18433,#18434,#18435,#18436,#18437,#18438,#18439,#18440,#18441,
#18442,#18443,#18444,#18445,#18446,#18447,#18448,#18449),(#18450,#18451,
#18452,#18453,#18454,#18455,#18456,#18457,#18458,#18459,#18460,#18461,#18462,
#18463,#18464,#18465,#18466,#18467,#18468,#18469,#18470,#18471,#18472,#18473,
#18474,#18475,#18476,#18477,#18478,#18479,#18480,#18481,#18482,#18483,#18484,
#18485,#18486,#18487,#18488,#18489,#18490,#18491,#18492,#18493,#18494,#18495,
#18496,#18497,#18498,#18499,#18500,#18501,#18502,#18503,#18504,#18505,#18506,
#18507,#18508,#18509,#18510,#18511,#18512,#18513,#18514,#18515,#18516,#18517,
#18518,#18519,#18520,#18521,#18522,#18523,#18524,#18525,#18526,#18527,#18528,
#18529,#18530,#18531,#18532,#18533,#18534,#18535,#18536,#18537,#18538,#18539,
#18540,#18541,#18542,#18543,#18544,#18545,#18546,#18547,#18548,#18549,#18550,
#18551,#18552,#18553,#18554,#18555,#18556,#18557,#18558,#18559,#18560,#18561),
(#18562,#18563,#18564,#18565,#18566,#18567,#18568,#18569,#18570,#18571,
#18572,#18573,#18574,#18575,#18576,#18577,#18578,#18579,#18580,#18581,#18582,
#18583,#18584,#18585,#18586,#18587,#18588,#18589,#18590,#18591,#18592,#18593,
#18594,#18595,#18596,#18597,#18598,#18599,#18600,#18601,#18602,#18603,#18604,
#18605,#18606,#18607,#18608,#18609,#18610,#18611,#18612,#18613,#18614,#18615,
#18616,#18617,#18618,#18619,#18620,#18621,#18622,#18623,#18624,#18625,#18626,
#18627,#18628,#18629,#18630,#18631,#18632,#18633,#18634,#18635,#18636,#18637,
#18638,#18639,#18640,#18641,#18642,#18643,#18644,#18645,#18646,#18647,#18648,
#18649,#18650,#18651,#18652,#18653,#18654,#18655,#18656,#18657,#18658,#18659,
#18660,#18661,#18662,#18663,#18664,#18665,#18666,#18667,#18668,#18669,#18670,
#18671,#18672,#18673),(#18674,#18675,#18676,#18677,#18678,#18679,#18680,
#18681,#18682,#18683,#18684,#18685,#18686,#18687,#18688,#18689,#18690,#18691,
#18692,#18693,#18694,#18695,#18696,#18697,#18698,#18699,#18700,#18701,#18702,
#18703,#18704,#18705,#18706,#18707,#18708,#18709,#18710,#18711,#18712,#18713,
#18714,#18715,#18716,#18717,#18718,#18719,#18720,#18721,#18722,#18723,#18724,
#18725,#18726,#18727,#18728,#18729,#18730,#18731,#18732,#18733,#18734,#18735,
#18736,#18737,#18738,#18739,#18740,#18741,#18742,#18743,#18744,#18745,#18746,
#18747,#18748,#18749,#18750,#18751,#18752,#18753,#18754,#18755,#18756,#18757,
#18758,#18759,#18760,#18761,#18762,#18763,#18764,#18765,#18766,#18767,#18768,
#18769,#18770,#18771,#18772,#18773,#18774,#18775,#18776,#18777,#18778,#18779,
#18780,#18781,#18782,#18783,#18784,#18785)),.UNSPECIFIED.,.F.,.F.,.F.,(4,
4),(4,1,1,1,1,1,1,1,1,1,1,1,1,1,1,1,1,1,1,1,1,1,1,1,1,1,1,1,1,1,1,1,1,1,
1,1,1,1,1,1,1,1,1,1,1,1,1,1,1,1,1,1,1,1,1,1,1,1,1,1,1,1,1,1,1,1,1,1,1,1,
1,1,1,1,1,1,1,1,1,1,1,1,1,1,1,1,1,1,1,1,1,1,1,1,1,1,1,1,1,1,1,1,1,1,1,1,
1,1,1,4),(0.,0.064201349933888),(14.3984001269718,15.3968505408716,16.3953009547714,
17.3937513686712,18.3922017825711,19.3906521964709,20.3891026103707,21.3875530242706,
22.3860034381704,23.3844538520702,24.38290426597,25.3813546798699,26.3798050937697,
27.3782555076695,28.3767059215694,29.3751563354692,30.373606749369,31.3720571632688,
32.3705075771687,33.3689579910685,34.3674084049683,35.3658588188682,36.364309232768,
37.3627596466678,38.3612100605677,39.3596604744675,40.3581108883673,41.3565613022671,
42.355011716167,43.3534621300668,44.3519125439666,45.3503629578665,46.3488133717663,
47.3472637856661,48.3457141995659,49.3441646134658,50.3426150273656,51.3410654412654,
52.3395158551653,53.3379662690651,54.3364166829649,55.3348670968648,56.3333175107646,
57.3317679246644,58.3302183385642,59.3286687524641,60.3271191663639,61.3255695802637,
62.3240199941636,63.3224704080634,64.3209208219632,65.319371235863,66.3178216497629,
67.3162720636627,68.3147224775625,69.3131728914624,70.3116233053622,71.310073719262,
72.3085241331619,73.3069745470617,74.3054249609615,75.3038753748613,76.3023257887612,
77.300776202661,78.2992266165608,79.2976770304607,80.2961274443605,81.2945778582603,
82.2930282721601,83.29147868606,84.2899290999598,85.2883795138596,86.2868299277595,
87.2852803416593,88.2837307555591,89.282181169459,90.2806315833588,91.2790819972586,
92.2775324111584,93.2759828250583,94.2744332389581,95.2728836528579,96.2713340667578,
97.2697844806576,98.2682348945574,99.2666853084572,100.265135722357,101.263586136257,
102.262036550157,103.260486964057,104.258937377956,105.257387791856,106.255838205756,
107.254288619656,108.252739033556,109.251189447456,110.249639861355,111.248090275255,
112.246540689155,113.244991103055,114.243441516955,115.241891930855,116.240342344754,
117.238792758654,118.237243172554,119.235693586454,120.234144000354,121.232594414253,
122.231044828153,123.229495242053),.UNSPECIFIED.);
#297=B_SPLINE_SURFACE_WITH_KNOTS('',3,3,((#19108,#19109,#19110,#19111,#19112,
#19113,#19114,#19115,#19116,#19117,#19118,#19119,#19120,#19121,#19122,#19123,
#19124,#19125,#19126,#19127,#19128,#19129,#19130,#19131,#19132,#19133,#19134,
#19135,#19136,#19137,#19138,#19139,#19140,#19141,#19142,#19143,#19144,#19145,
#19146,#19147,#19148,#19149,#19150,#19151,#19152,#19153,#19154,#19155,#19156,
#19157,#19158,#19159,#19160,#19161,#19162,#19163,#19164,#19165,#19166,#19167,
#19168,#19169,#19170,#19171,#19172,#19173,#19174,#19175,#19176,#19177,#19178,
#19179,#19180,#19181,#19182,#19183,#19184,#19185,#19186,#19187,#19188,#19189,
#19190,#19191,#19192,#19193,#19194,#19195,#19196,#19197,#19198,#19199,#19200,
#19201,#19202,#19203,#19204,#19205,#19206,#19207,#19208,#19209,#19210,#19211,
#19212,#19213,#19214,#19215,#19216,#19217,#19218,#19219),(#19220,#19221,
#19222,#19223,#19224,#19225,#19226,#19227,#19228,#19229,#19230,#19231,#19232,
#19233,#19234,#19235,#19236,#19237,#19238,#19239,#19240,#19241,#19242,#19243,
#19244,#19245,#19246,#19247,#19248,#19249,#19250,#19251,#19252,#19253,#19254,
#19255,#19256,#19257,#19258,#19259,#19260,#19261,#19262,#19263,#19264,#19265,
#19266,#19267,#19268,#19269,#19270,#19271,#19272,#19273,#19274,#19275,#19276,
#19277,#19278,#19279,#19280,#19281,#19282,#19283,#19284,#19285,#19286,#19287,
#19288,#19289,#19290,#19291,#19292,#19293,#19294,#19295,#19296,#19297,#19298,
#19299,#19300,#19301,#19302,#19303,#19304,#19305,#19306,#19307,#19308,#19309,
#19310,#19311,#19312,#19313,#19314,#19315,#19316,#19317,#19318,#19319,#19320,
#19321,#19322,#19323,#19324,#19325,#19326,#19327,#19328,#19329,#19330,#19331),
(#19332,#19333,#19334,#19335,#19336,#19337,#19338,#19339,#19340,#19341,
#19342,#19343,#19344,#19345,#19346,#19347,#19348,#19349,#19350,#19351,#19352,
#19353,#19354,#19355,#19356,#19357,#19358,#19359,#19360,#19361,#19362,#19363,
#19364,#19365,#19366,#19367,#19368,#19369,#19370,#19371,#19372,#19373,#19374,
#19375,#19376,#19377,#19378,#19379,#19380,#19381,#19382,#19383,#19384,#19385,
#19386,#19387,#19388,#19389,#19390,#19391,#19392,#19393,#19394,#19395,#19396,
#19397,#19398,#19399,#19400,#19401,#19402,#19403,#19404,#19405,#19406,#19407,
#19408,#19409,#19410,#19411,#19412,#19413,#19414,#19415,#19416,#19417,#19418,
#19419,#19420,#19421,#19422,#19423,#19424,#19425,#19426,#19427,#19428,#19429,
#19430,#19431,#19432,#19433,#19434,#19435,#19436,#19437,#19438,#19439,#19440,
#19441,#19442,#19443),(#19444,#19445,#19446,#19447,#19448,#19449,#19450,
#19451,#19452,#19453,#19454,#19455,#19456,#19457,#19458,#19459,#19460,#19461,
#19462,#19463,#19464,#19465,#19466,#19467,#19468,#19469,#19470,#19471,#19472,
#19473,#19474,#19475,#19476,#19477,#19478,#19479,#19480,#19481,#19482,#19483,
#19484,#19485,#19486,#19487,#19488,#19489,#19490,#19491,#19492,#19493,#19494,
#19495,#19496,#19497,#19498,#19499,#19500,#19501,#19502,#19503,#19504,#19505,
#19506,#19507,#19508,#19509,#19510,#19511,#19512,#19513,#19514,#19515,#19516,
#19517,#19518,#19519,#19520,#19521,#19522,#19523,#19524,#19525,#19526,#19527,
#19528,#19529,#19530,#19531,#19532,#19533,#19534,#19535,#19536,#19537,#19538,
#19539,#19540,#19541,#19542,#19543,#19544,#19545,#19546,#19547,#19548,#19549,
#19550,#19551,#19552,#19553,#19554,#19555)),.UNSPECIFIED.,.F.,.F.,.F.,(4,
4),(4,1,1,1,1,1,1,1,1,1,1,1,1,1,1,1,1,1,1,1,1,1,1,1,1,1,1,1,1,1,1,1,1,1,
1,1,1,1,1,1,1,1,1,1,1,1,1,1,1,1,1,1,1,1,1,1,1,1,1,1,1,1,1,1,1,1,1,1,1,1,
1,1,1,1,1,1,1,1,1,1,1,1,1,1,1,1,1,1,1,1,1,1,1,1,1,1,1,1,1,1,1,1,1,1,1,1,
1,1,1,4),(0.,0.064201349933888),(11.8589888623077,12.8574392762076,13.8558896901074,
14.8543401040072,15.852790517907,16.8512409318069,17.8496913457067,18.8481417596065,
19.8465921735064,20.8450425874062,21.843493001306,22.8419434152058,23.8403938291057,
24.8388442430055,25.8372946569053,26.8357450708052,27.834195484705,28.8326458986048,
29.8310963125047,30.8295467264045,31.8279971403043,32.8264475542041,33.824897968104,
34.8233483820038,35.8217987959036,36.8202492098035,37.8186996237033,38.8171500376031,
39.8156004515029,40.8140508654028,41.8125012793026,42.8109516932024,43.8094021071023,
44.8078525210021,45.8063029349019,46.8047533488018,47.8032037627016,48.8016541766014,
49.8001045905012,50.7985550044011,51.7970054183009,52.7954558322007,53.7939062461006,
54.7923566600004,55.7908070739002,56.7892574878,57.7877079016999,58.7861583155997,
59.7846087294995,60.7830591433994,61.7815095572992,62.779959971199,63.7784103850989,
64.7768607989987,65.7753112128985,66.7737616267983,67.7722120406982,68.770662454598,
69.7691128684978,70.7675632823977,71.7660136962975,72.7644641101973,73.7629145240972,
74.761364937997,75.7598153518968,76.7582657657966,77.7567161796965,78.7551665935963,
79.7536170074961,80.752067421396,81.7505178352958,82.7489682491956,83.7474186630954,
84.7458690769953,85.7443194908951,86.7427699047949,87.7412203186948,88.7396707325946,
89.7381211464944,90.7365715603943,91.7350219742941,92.7334723881939,93.7319228020937,
94.7303732159936,95.7288236298934,96.7272740437932,97.7257244576931,98.7241748715929,
99.7226252854927,100.721075699393,101.719526113292,102.717976527192,103.716426941092,
104.714877354992,105.713327768892,106.711778182792,107.710228596691,108.708679010591,
109.707129424491,110.705579838391,111.704030252291,112.70248066619,113.70093108009,
114.69938149399,115.69783190789,116.69628232179,117.69473273569,118.693183149589,
119.691633563489,120.690083977389),.UNSPECIFIED.);
#298=B_SPLINE_SURFACE_WITH_KNOTS('',3,3,((#19678,#19679,#19680,#19681,#19682,
#19683,#19684,#19685,#19686,#19687,#19688,#19689,#19690,#19691,#19692,#19693,
#19694,#19695,#19696,#19697,#19698,#19699,#19700,#19701,#19702,#19703,#19704,
#19705,#19706,#19707,#19708,#19709,#19710,#19711,#19712,#19713,#19714,#19715,
#19716,#19717,#19718,#19719,#19720,#19721,#19722,#19723,#19724,#19725,#19726,
#19727,#19728,#19729,#19730,#19731,#19732,#19733,#19734,#19735,#19736,#19737,
#19738,#19739,#19740,#19741,#19742,#19743,#19744,#19745,#19746,#19747,#19748,
#19749,#19750,#19751,#19752,#19753,#19754,#19755,#19756,#19757,#19758,#19759,
#19760,#19761,#19762,#19763,#19764,#19765,#19766,#19767,#19768,#19769,#19770,
#19771,#19772,#19773,#19774,#19775,#19776,#19777,#19778,#19779,#19780,#19781,
#19782,#19783,#19784,#19785,#19786,#19787,#19788,#19789),(#19790,#19791,
#19792,#19793,#19794,#19795,#19796,#19797,#19798,#19799,#19800,#19801,#19802,
#19803,#19804,#19805,#19806,#19807,#19808,#19809,#19810,#19811,#19812,#19813,
#19814,#19815,#19816,#19817,#19818,#19819,#19820,#19821,#19822,#19823,#19824,
#19825,#19826,#19827,#19828,#19829,#19830,#19831,#19832,#19833,#19834,#19835,
#19836,#19837,#19838,#19839,#19840,#19841,#19842,#19843,#19844,#19845,#19846,
#19847,#19848,#19849,#19850,#19851,#19852,#19853,#19854,#19855,#19856,#19857,
#19858,#19859,#19860,#19861,#19862,#19863,#19864,#19865,#19866,#19867,#19868,
#19869,#19870,#19871,#19872,#19873,#19874,#19875,#19876,#19877,#19878,#19879,
#19880,#19881,#19882,#19883,#19884,#19885,#19886,#19887,#19888,#19889,#19890,
#19891,#19892,#19893,#19894,#19895,#19896,#19897,#19898,#19899,#19900,#19901),
(#19902,#19903,#19904,#19905,#19906,#19907,#19908,#19909,#19910,#19911,
#19912,#19913,#19914,#19915,#19916,#19917,#19918,#19919,#19920,#19921,#19922,
#19923,#19924,#19925,#19926,#19927,#19928,#19929,#19930,#19931,#19932,#19933,
#19934,#19935,#19936,#19937,#19938,#19939,#19940,#19941,#19942,#19943,#19944,
#19945,#19946,#19947,#19948,#19949,#19950,#19951,#19952,#19953,#19954,#19955,
#19956,#19957,#19958,#19959,#19960,#19961,#19962,#19963,#19964,#19965,#19966,
#19967,#19968,#19969,#19970,#19971,#19972,#19973,#19974,#19975,#19976,#19977,
#19978,#19979,#19980,#19981,#19982,#19983,#19984,#19985,#19986,#19987,#19988,
#19989,#19990,#19991,#19992,#19993,#19994,#19995,#19996,#19997,#19998,#19999,
#20000,#20001,#20002,#20003,#20004,#20005,#20006,#20007,#20008,#20009,#20010,
#20011,#20012,#20013),(#20014,#20015,#20016,#20017,#20018,#20019,#20020,
#20021,#20022,#20023,#20024,#20025,#20026,#20027,#20028,#20029,#20030,#20031,
#20032,#20033,#20034,#20035,#20036,#20037,#20038,#20039,#20040,#20041,#20042,
#20043,#20044,#20045,#20046,#20047,#20048,#20049,#20050,#20051,#20052,#20053,
#20054,#20055,#20056,#20057,#20058,#20059,#20060,#20061,#20062,#20063,#20064,
#20065,#20066,#20067,#20068,#20069,#20070,#20071,#20072,#20073,#20074,#20075,
#20076,#20077,#20078,#20079,#20080,#20081,#20082,#20083,#20084,#20085,#20086,
#20087,#20088,#20089,#20090,#20091,#20092,#20093,#20094,#20095,#20096,#20097,
#20098,#20099,#20100,#20101,#20102,#20103,#20104,#20105,#20106,#20107,#20108,
#20109,#20110,#20111,#20112,#20113,#20114,#20115,#20116,#20117,#20118,#20119,
#20120,#20121,#20122,#20123,#20124,#20125)),.UNSPECIFIED.,.F.,.F.,.F.,(4,
4),(4,1,1,1,1,1,1,1,1,1,1,1,1,1,1,1,1,1,1,1,1,1,1,1,1,1,1,1,1,1,1,1,1,1,
1,1,1,1,1,1,1,1,1,1,1,1,1,1,1,1,1,1,1,1,1,1,1,1,1,1,1,1,1,1,1,1,1,1,1,1,
1,1,1,1,1,1,1,1,1,1,1,1,1,1,1,1,1,1,1,1,1,1,1,1,1,1,1,1,1,1,1,1,1,1,1,1,
1,1,1,4),(0.,0.064201349933888),(14.3984001269717,15.3968505408716,16.3953009547714,
17.3937513686712,18.3922017825711,19.3906521964709,20.3891026103707,21.3875530242705,
22.3860034381704,23.3844538520702,24.38290426597,25.3813546798699,26.3798050937697,
27.3782555076695,28.3767059215694,29.3751563354692,30.373606749369,31.3720571632688,
32.3705075771687,33.3689579910685,34.3674084049683,35.3658588188682,36.364309232768,
37.3627596466678,38.3612100605677,39.3596604744675,40.3581108883673,41.3565613022671,
42.355011716167,43.3534621300668,44.3519125439666,45.3503629578665,46.3488133717663,
47.3472637856661,48.3457141995659,49.3441646134658,50.3426150273656,51.3410654412654,
52.3395158551653,53.3379662690651,54.3364166829649,55.3348670968648,56.3333175107646,
57.3317679246644,58.3302183385642,59.3286687524641,60.3271191663639,61.3255695802637,
62.3240199941636,63.3224704080634,64.3209208219632,65.319371235863,66.3178216497629,
67.3162720636627,68.3147224775625,69.3131728914624,70.3116233053622,71.310073719262,
72.3085241331619,73.3069745470617,74.3054249609615,75.3038753748613,76.3023257887612,
77.300776202661,78.2992266165608,79.2976770304606,80.2961274443605,81.2945778582603,
82.2930282721601,83.29147868606,84.2899290999598,85.2883795138596,86.2868299277595,
87.2852803416593,88.2837307555591,89.282181169459,90.2806315833588,91.2790819972586,
92.2775324111584,93.2759828250583,94.2744332389581,95.2728836528579,96.2713340667578,
97.2697844806576,98.2682348945574,99.2666853084572,100.265135722357,101.263586136257,
102.262036550157,103.260486964057,104.258937377956,105.257387791856,106.255838205756,
107.254288619656,108.252739033556,109.251189447456,110.249639861355,111.248090275255,
112.246540689155,113.244991103055,114.243441516955,115.241891930855,116.240342344754,
117.238792758654,118.237243172554,119.235693586454,120.234144000354,121.232594414253,
122.231044828153,123.229495242053),.UNSPECIFIED.);
#299=B_SPLINE_SURFACE_WITH_KNOTS('',3,3,((#20448,#20449,#20450,#20451,#20452,
#20453,#20454,#20455,#20456,#20457,#20458,#20459,#20460,#20461,#20462,#20463,
#20464,#20465,#20466,#20467,#20468,#20469,#20470,#20471,#20472,#20473,#20474,
#20475,#20476,#20477,#20478,#20479,#20480,#20481,#20482,#20483,#20484,#20485,
#20486,#20487,#20488,#20489,#20490,#20491,#20492,#20493,#20494,#20495,#20496,
#20497,#20498,#20499,#20500,#20501,#20502,#20503,#20504,#20505,#20506,#20507,
#20508,#20509,#20510,#20511,#20512,#20513,#20514,#20515,#20516,#20517,#20518,
#20519,#20520,#20521,#20522,#20523,#20524,#20525,#20526,#20527,#20528,#20529,
#20530,#20531,#20532,#20533,#20534,#20535,#20536,#20537,#20538,#20539,#20540,
#20541,#20542,#20543,#20544,#20545,#20546,#20547,#20548,#20549,#20550,#20551,
#20552,#20553,#20554,#20555,#20556,#20557,#20558,#20559),(#20560,#20561,
#20562,#20563,#20564,#20565,#20566,#20567,#20568,#20569,#20570,#20571,#20572,
#20573,#20574,#20575,#20576,#20577,#20578,#20579,#20580,#20581,#20582,#20583,
#20584,#20585,#20586,#20587,#20588,#20589,#20590,#20591,#20592,#20593,#20594,
#20595,#20596,#20597,#20598,#20599,#20600,#20601,#20602,#20603,#20604,#20605,
#20606,#20607,#20608,#20609,#20610,#20611,#20612,#20613,#20614,#20615,#20616,
#20617,#20618,#20619,#20620,#20621,#20622,#20623,#20624,#20625,#20626,#20627,
#20628,#20629,#20630,#20631,#20632,#20633,#20634,#20635,#20636,#20637,#20638,
#20639,#20640,#20641,#20642,#20643,#20644,#20645,#20646,#20647,#20648,#20649,
#20650,#20651,#20652,#20653,#20654,#20655,#20656,#20657,#20658,#20659,#20660,
#20661,#20662,#20663,#20664,#20665,#20666,#20667,#20668,#20669,#20670,#20671),
(#20672,#20673,#20674,#20675,#20676,#20677,#20678,#20679,#20680,#20681,
#20682,#20683,#20684,#20685,#20686,#20687,#20688,#20689,#20690,#20691,#20692,
#20693,#20694,#20695,#20696,#20697,#20698,#20699,#20700,#20701,#20702,#20703,
#20704,#20705,#20706,#20707,#20708,#20709,#20710,#20711,#20712,#20713,#20714,
#20715,#20716,#20717,#20718,#20719,#20720,#20721,#20722,#20723,#20724,#20725,
#20726,#20727,#20728,#20729,#20730,#20731,#20732,#20733,#20734,#20735,#20736,
#20737,#20738,#20739,#20740,#20741,#20742,#20743,#20744,#20745,#20746,#20747,
#20748,#20749,#20750,#20751,#20752,#20753,#20754,#20755,#20756,#20757,#20758,
#20759,#20760,#20761,#20762,#20763,#20764,#20765,#20766,#20767,#20768,#20769,
#20770,#20771,#20772,#20773,#20774,#20775,#20776,#20777,#20778,#20779,#20780,
#20781,#20782,#20783),(#20784,#20785,#20786,#20787,#20788,#20789,#20790,
#20791,#20792,#20793,#20794,#20795,#20796,#20797,#20798,#20799,#20800,#20801,
#20802,#20803,#20804,#20805,#20806,#20807,#20808,#20809,#20810,#20811,#20812,
#20813,#20814,#20815,#20816,#20817,#20818,#20819,#20820,#20821,#20822,#20823,
#20824,#20825,#20826,#20827,#20828,#20829,#20830,#20831,#20832,#20833,#20834,
#20835,#20836,#20837,#20838,#20839,#20840,#20841,#20842,#20843,#20844,#20845,
#20846,#20847,#20848,#20849,#20850,#20851,#20852,#20853,#20854,#20855,#20856,
#20857,#20858,#20859,#20860,#20861,#20862,#20863,#20864,#20865,#20866,#20867,
#20868,#20869,#20870,#20871,#20872,#20873,#20874,#20875,#20876,#20877,#20878,
#20879,#20880,#20881,#20882,#20883,#20884,#20885,#20886,#20887,#20888,#20889,
#20890,#20891,#20892,#20893,#20894,#20895)),.UNSPECIFIED.,.F.,.F.,.F.,(4,
4),(4,1,1,1,1,1,1,1,1,1,1,1,1,1,1,1,1,1,1,1,1,1,1,1,1,1,1,1,1,1,1,1,1,1,
1,1,1,1,1,1,1,1,1,1,1,1,1,1,1,1,1,1,1,1,1,1,1,1,1,1,1,1,1,1,1,1,1,1,1,1,
1,1,1,1,1,1,1,1,1,1,1,1,1,1,1,1,1,1,1,1,1,1,1,1,1,1,1,1,1,1,1,1,1,1,1,1,
1,1,1,4),(0.,0.064201349933888),(11.8589888623077,12.8574392762076,13.8558896901074,
14.8543401040072,15.852790517907,16.8512409318069,17.8496913457067,18.8481417596065,
19.8465921735064,20.8450425874062,21.843493001306,22.8419434152059,23.8403938291057,
24.8388442430055,25.8372946569053,26.8357450708052,27.834195484705,28.8326458986048,
29.8310963125047,30.8295467264045,31.8279971403043,32.8264475542042,33.824897968104,
34.8233483820038,35.8217987959036,36.8202492098035,37.8186996237033,38.8171500376031,
39.815600451503,40.8140508654028,41.8125012793026,42.8109516932024,43.8094021071023,
44.8078525210021,45.8063029349019,46.8047533488018,47.8032037627016,48.8016541766014,
49.8001045905012,50.7985550044011,51.7970054183009,52.7954558322007,53.7939062461006,
54.7923566600004,55.7908070739002,56.7892574878001,57.7877079016999,58.7861583155997,
59.7846087294995,60.7830591433994,61.7815095572992,62.779959971199,63.7784103850989,
64.7768607989987,65.7753112128985,66.7737616267983,67.7722120406982,68.770662454598,
69.7691128684978,70.7675632823977,71.7660136962975,72.7644641101973,73.7629145240972,
74.761364937997,75.7598153518968,76.7582657657966,77.7567161796965,78.7551665935963,
79.7536170074961,80.7520674213959,81.7505178352958,82.7489682491956,83.7474186630954,
84.7458690769953,85.7443194908951,86.7427699047949,87.7412203186948,88.7396707325946,
89.7381211464944,90.7365715603942,91.7350219742941,92.7334723881939,93.7319228020937,
94.7303732159936,95.7288236298934,96.7272740437932,97.725724457693,98.7241748715929,
99.7226252854927,100.721075699393,101.719526113292,102.717976527192,103.716426941092,
104.714877354992,105.713327768892,106.711778182792,107.710228596691,108.708679010591,
109.707129424491,110.705579838391,111.704030252291,112.70248066619,113.70093108009,
114.69938149399,115.69783190789,116.69628232179,117.69473273569,118.693183149589,
119.691633563489,120.690083977389),.UNSPECIFIED.);
#300=B_SPLINE_SURFACE_WITH_KNOTS('',3,3,((#21018,#21019,#21020,#21021,#21022,
#21023,#21024,#21025,#21026,#21027,#21028,#21029,#21030,#21031,#21032,#21033,
#21034,#21035,#21036,#21037,#21038,#21039,#21040,#21041,#21042,#21043,#21044,
#21045,#21046,#21047,#21048,#21049,#21050,#21051,#21052,#21053,#21054,#21055,
#21056,#21057,#21058,#21059,#21060,#21061,#21062,#21063,#21064,#21065,#21066,
#21067,#21068,#21069,#21070,#21071,#21072,#21073,#21074,#21075,#21076,#21077,
#21078,#21079,#21080,#21081,#21082,#21083,#21084,#21085,#21086,#21087,#21088,
#21089,#21090,#21091,#21092,#21093,#21094,#21095,#21096,#21097,#21098,#21099,
#21100,#21101,#21102,#21103,#21104,#21105,#21106,#21107,#21108,#21109,#21110,
#21111,#21112,#21113,#21114,#21115,#21116,#21117,#21118,#21119,#21120,#21121,
#21122,#21123,#21124,#21125,#21126,#21127,#21128,#21129),(#21130,#21131,
#21132,#21133,#21134,#21135,#21136,#21137,#21138,#21139,#21140,#21141,#21142,
#21143,#21144,#21145,#21146,#21147,#21148,#21149,#21150,#21151,#21152,#21153,
#21154,#21155,#21156,#21157,#21158,#21159,#21160,#21161,#21162,#21163,#21164,
#21165,#21166,#21167,#21168,#21169,#21170,#21171,#21172,#21173,#21174,#21175,
#21176,#21177,#21178,#21179,#21180,#21181,#21182,#21183,#21184,#21185,#21186,
#21187,#21188,#21189,#21190,#21191,#21192,#21193,#21194,#21195,#21196,#21197,
#21198,#21199,#21200,#21201,#21202,#21203,#21204,#21205,#21206,#21207,#21208,
#21209,#21210,#21211,#21212,#21213,#21214,#21215,#21216,#21217,#21218,#21219,
#21220,#21221,#21222,#21223,#21224,#21225,#21226,#21227,#21228,#21229,#21230,
#21231,#21232,#21233,#21234,#21235,#21236,#21237,#21238,#21239,#21240,#21241),
(#21242,#21243,#21244,#21245,#21246,#21247,#21248,#21249,#21250,#21251,
#21252,#21253,#21254,#21255,#21256,#21257,#21258,#21259,#21260,#21261,#21262,
#21263,#21264,#21265,#21266,#21267,#21268,#21269,#21270,#21271,#21272,#21273,
#21274,#21275,#21276,#21277,#21278,#21279,#21280,#21281,#21282,#21283,#21284,
#21285,#21286,#21287,#21288,#21289,#21290,#21291,#21292,#21293,#21294,#21295,
#21296,#21297,#21298,#21299,#21300,#21301,#21302,#21303,#21304,#21305,#21306,
#21307,#21308,#21309,#21310,#21311,#21312,#21313,#21314,#21315,#21316,#21317,
#21318,#21319,#21320,#21321,#21322,#21323,#21324,#21325,#21326,#21327,#21328,
#21329,#21330,#21331,#21332,#21333,#21334,#21335,#21336,#21337,#21338,#21339,
#21340,#21341,#21342,#21343,#21344,#21345,#21346,#21347,#21348,#21349,#21350,
#21351,#21352,#21353),(#21354,#21355,#21356,#21357,#21358,#21359,#21360,
#21361,#21362,#21363,#21364,#21365,#21366,#21367,#21368,#21369,#21370,#21371,
#21372,#21373,#21374,#21375,#21376,#21377,#21378,#21379,#21380,#21381,#21382,
#21383,#21384,#21385,#21386,#21387,#21388,#21389,#21390,#21391,#21392,#21393,
#21394,#21395,#21396,#21397,#21398,#21399,#21400,#21401,#21402,#21403,#21404,
#21405,#21406,#21407,#21408,#21409,#21410,#21411,#21412,#21413,#21414,#21415,
#21416,#21417,#21418,#21419,#21420,#21421,#21422,#21423,#21424,#21425,#21426,
#21427,#21428,#21429,#21430,#21431,#21432,#21433,#21434,#21435,#21436,#21437,
#21438,#21439,#21440,#21441,#21442,#21443,#21444,#21445,#21446,#21447,#21448,
#21449,#21450,#21451,#21452,#21453,#21454,#21455,#21456,#21457,#21458,#21459,
#21460,#21461,#21462,#21463,#21464,#21465)),.UNSPECIFIED.,.F.,.F.,.F.,(4,
4),(4,1,1,1,1,1,1,1,1,1,1,1,1,1,1,1,1,1,1,1,1,1,1,1,1,1,1,1,1,1,1,1,1,1,
1,1,1,1,1,1,1,1,1,1,1,1,1,1,1,1,1,1,1,1,1,1,1,1,1,1,1,1,1,1,1,1,1,1,1,1,
1,1,1,1,1,1,1,1,1,1,1,1,1,1,1,1,1,1,1,1,1,1,1,1,1,1,1,1,1,1,1,1,1,1,1,1,
1,1,1,4),(0.,0.064201349933888),(14.3984001269718,15.3968505408716,16.3953009547714,
17.3937513686712,18.3922017825711,19.3906521964709,20.3891026103707,21.3875530242706,
22.3860034381704,23.3844538520702,24.38290426597,25.3813546798699,26.3798050937697,
27.3782555076695,28.3767059215694,29.3751563354692,30.373606749369,31.3720571632689,
32.3705075771687,33.3689579910685,34.3674084049683,35.3658588188682,36.364309232768,
37.3627596466678,38.3612100605677,39.3596604744675,40.3581108883673,41.3565613022671,
42.355011716167,43.3534621300668,44.3519125439666,45.3503629578665,46.3488133717663,
47.3472637856661,48.345714199566,49.3441646134658,50.3426150273656,51.3410654412654,
52.3395158551653,53.3379662690651,54.3364166829649,55.3348670968648,56.3333175107646,
57.3317679246644,58.3302183385643,59.3286687524641,60.3271191663639,61.3255695802637,
62.3240199941636,63.3224704080634,64.3209208219632,65.3193712358631,66.3178216497629,
67.3162720636627,68.3147224775625,69.3131728914624,70.3116233053622,71.310073719262,
72.3085241331619,73.3069745470617,74.3054249609615,75.3038753748613,76.3023257887612,
77.300776202661,78.2992266165608,79.2976770304607,80.2961274443605,81.2945778582603,
82.2930282721602,83.29147868606,84.2899290999598,85.2883795138596,86.2868299277595,
87.2852803416593,88.2837307555591,89.282181169459,90.2806315833588,91.2790819972586,
92.2775324111584,93.2759828250583,94.2744332389581,95.2728836528579,96.2713340667578,
97.2697844806576,98.2682348945574,99.2666853084573,100.265135722357,101.263586136257,
102.262036550157,103.260486964057,104.258937377956,105.257387791856,106.255838205756,
107.254288619656,108.252739033556,109.251189447456,110.249639861355,111.248090275255,
112.246540689155,113.244991103055,114.243441516955,115.241891930855,116.240342344754,
117.238792758654,118.237243172554,119.235693586454,120.234144000354,121.232594414253,
122.231044828153,123.229495242053),.UNSPECIFIED.);
#301=B_SPLINE_SURFACE_WITH_KNOTS('',3,3,((#23063,#23064,#23065,#23066,#23067,
#23068,#23069,#23070,#23071,#23072,#23073,#23074,#23075,#23076,#23077,#23078,
#23079,#23080,#23081,#23082,#23083,#23084,#23085,#23086,#23087,#23088,#23089,
#23090,#23091,#23092,#23093,#23094,#23095,#23096,#23097,#23098,#23099,#23100,
#23101,#23102,#23103,#23104,#23105,#23106,#23107,#23108,#23109,#23110,#23111,
#23112,#23113,#23114,#23115,#23116,#23117,#23118,#23119,#23120,#23121,#23122,
#23123,#23124,#23125,#23126,#23127,#23128,#23129,#23130,#23131,#23132,#23133,
#23134,#23135,#23136,#23137,#23138,#23139,#23140,#23141,#23142,#23143,#23144,
#23145,#23146,#23147,#23148,#23149,#23150,#23151,#23152,#23153,#23154,#23155,
#23156,#23157,#23158,#23159,#23160,#23161,#23162,#23163,#23164,#23165,#23166),
(#23167,#23168,#23169,#23170,#23171,#23172,#23173,#23174,#23175,#23176,
#23177,#23178,#23179,#23180,#23181,#23182,#23183,#23184,#23185,#23186,#23187,
#23188,#23189,#23190,#23191,#23192,#23193,#23194,#23195,#23196,#23197,#23198,
#23199,#23200,#23201,#23202,#23203,#23204,#23205,#23206,#23207,#23208,#23209,
#23210,#23211,#23212,#23213,#23214,#23215,#23216,#23217,#23218,#23219,#23220,
#23221,#23222,#23223,#23224,#23225,#23226,#23227,#23228,#23229,#23230,#23231,
#23232,#23233,#23234,#23235,#23236,#23237,#23238,#23239,#23240,#23241,#23242,
#23243,#23244,#23245,#23246,#23247,#23248,#23249,#23250,#23251,#23252,#23253,
#23254,#23255,#23256,#23257,#23258,#23259,#23260,#23261,#23262,#23263,#23264,
#23265,#23266,#23267,#23268,#23269,#23270),(#23271,#23272,#23273,#23274,
#23275,#23276,#23277,#23278,#23279,#23280,#23281,#23282,#23283,#23284,#23285,
#23286,#23287,#23288,#23289,#23290,#23291,#23292,#23293,#23294,#23295,#23296,
#23297,#23298,#23299,#23300,#23301,#23302,#23303,#23304,#23305,#23306,#23307,
#23308,#23309,#23310,#23311,#23312,#23313,#23314,#23315,#23316,#23317,#23318,
#23319,#23320,#23321,#23322,#23323,#23324,#23325,#23326,#23327,#23328,#23329,
#23330,#23331,#23332,#23333,#23334,#23335,#23336,#23337,#23338,#23339,#23340,
#23341,#23342,#23343,#23344,#23345,#23346,#23347,#23348,#23349,#23350,#23351,
#23352,#23353,#23354,#23355,#23356,#23357,#23358,#23359,#23360,#23361,#23362,
#23363,#23364,#23365,#23366,#23367,#23368,#23369,#23370,#23371,#23372,#23373,
#23374),(#23375,#23376,#23377,#23378,#23379,#23380,#23381,#23382,#23383,
#23384,#23385,#23386,#23387,#23388,#23389,#23390,#23391,#23392,#23393,#23394,
#23395,#23396,#23397,#23398,#23399,#23400,#23401,#23402,#23403,#23404,#23405,
#23406,#23407,#23408,#23409,#23410,#23411,#23412,#23413,#23414,#23415,#23416,
#23417,#23418,#23419,#23420,#23421,#23422,#23423,#23424,#23425,#23426,#23427,
#23428,#23429,#23430,#23431,#23432,#23433,#23434,#23435,#23436,#23437,#23438,
#23439,#23440,#23441,#23442,#23443,#23444,#23445,#23446,#23447,#23448,#23449,
#23450,#23451,#23452,#23453,#23454,#23455,#23456,#23457,#23458,#23459,#23460,
#23461,#23462,#23463,#23464,#23465,#23466,#23467,#23468,#23469,#23470,#23471,
#23472,#23473,#23474,#23475,#23476,#23477,#23478)),.UNSPECIFIED.,.F.,.F.,
 .F.,(4,4),(4,1,1,1,1,1,1,1,1,1,1,1,1,1,1,1,1,1,1,1,1,1,1,1,1,1,1,1,1,1,
1,1,1,1,1,1,1,1,1,1,1,1,1,1,1,1,1,1,1,1,1,1,1,1,1,1,1,1,1,1,1,1,1,1,1,1,
1,1,1,1,1,1,1,1,1,1,1,1,1,1,1,1,1,1,1,1,1,1,1,1,1,1,1,1,1,1,1,1,1,1,1,4),
(0.,0.0448889834294935),(11.8615800042566,12.8591085386932,13.8566370731298,
14.8541656075664,15.851694142003,16.8492226764396,17.8467512108762,18.8442797453128,
19.8418082797494,20.839336814186,21.8368653486226,22.8343938830592,23.8319224174958,
24.8294509519324,25.826979486369,26.8245080208056,27.8220365552422,28.8195650896788,
29.8170936241154,30.814622158552,31.8121506929886,32.8096792274252,33.8072077618618,
34.8047362962984,35.802264830735,36.7997933651716,37.7973218996082,38.7948504340448,
39.7923789684814,40.789907502918,41.7874360373546,42.7849645717912,43.7824931062278,
44.7800216406644,45.777550175101,46.7750787095376,47.7726072439742,48.7701357784108,
49.7676643128474,50.765192847284,51.7627213817206,52.7602499161572,53.7577784505938,
54.7553069850304,55.752835519467,56.7503640539036,57.7478925883402,58.7454211227768,
59.7429496572134,60.74047819165,61.7380067260866,62.7355352605232,63.7330637949598,
64.7305923293964,65.728120863833,66.7256493982696,67.7231779327062,68.7207064671428,
69.7182350015794,70.715763536016,71.7132920704526,72.7108206048892,73.7083491393258,
74.7058776737624,75.703406208199,76.7009347426356,77.6984632770722,78.6959918115088,
79.6935203459454,80.691048880382,81.6885774148186,82.6861059492552,83.6836344836918,
84.6811630181284,85.678691552565,86.6762200870016,87.6737486214382,88.6712771558748,
89.6688056903114,90.666334224748,91.6638627591846,92.6613912936212,93.6589198280577,
94.6564483624943,95.6539768969309,96.6515054313676,97.6490339658042,98.6465625002407,
99.6440910346773,100.641619569114,101.639148103551,102.636676637987,103.634205172424,
104.63173370686,105.629262241297,106.626790775734,107.62431931017,108.621847844607,
109.619376379043,110.61690491348,111.614433447917,112.611961982353),
 .UNSPECIFIED.);
#302=B_SPLINE_SURFACE_WITH_KNOTS('',3,3,((#23586,#23587,#23588,#23589,#23590,
#23591,#23592,#23593,#23594,#23595,#23596,#23597,#23598,#23599,#23600,#23601,
#23602,#23603,#23604,#23605,#23606,#23607,#23608,#23609,#23610,#23611,#23612,
#23613,#23614,#23615,#23616,#23617,#23618,#23619,#23620,#23621,#23622,#23623,
#23624,#23625,#23626,#23627,#23628,#23629,#23630,#23631,#23632,#23633,#23634,
#23635,#23636,#23637,#23638,#23639,#23640,#23641,#23642,#23643,#23644,#23645,
#23646,#23647,#23648,#23649,#23650,#23651,#23652,#23653,#23654,#23655,#23656,
#23657,#23658,#23659,#23660,#23661,#23662,#23663,#23664,#23665,#23666,#23667,
#23668,#23669,#23670,#23671,#23672,#23673,#23674,#23675,#23676,#23677,#23678,
#23679,#23680,#23681,#23682,#23683,#23684,#23685,#23686,#23687,#23688,#23689),
(#23690,#23691,#23692,#23693,#23694,#23695,#23696,#23697,#23698,#23699,
#23700,#23701,#23702,#23703,#23704,#23705,#23706,#23707,#23708,#23709,#23710,
#23711,#23712,#23713,#23714,#23715,#23716,#23717,#23718,#23719,#23720,#23721,
#23722,#23723,#23724,#23725,#23726,#23727,#23728,#23729,#23730,#23731,#23732,
#23733,#23734,#23735,#23736,#23737,#23738,#23739,#23740,#23741,#23742,#23743,
#23744,#23745,#23746,#23747,#23748,#23749,#23750,#23751,#23752,#23753,#23754,
#23755,#23756,#23757,#23758,#23759,#23760,#23761,#23762,#23763,#23764,#23765,
#23766,#23767,#23768,#23769,#23770,#23771,#23772,#23773,#23774,#23775,#23776,
#23777,#23778,#23779,#23780,#23781,#23782,#23783,#23784,#23785,#23786,#23787,
#23788,#23789,#23790,#23791,#23792,#23793),(#23794,#23795,#23796,#23797,
#23798,#23799,#23800,#23801,#23802,#23803,#23804,#23805,#23806,#23807,#23808,
#23809,#23810,#23811,#23812,#23813,#23814,#23815,#23816,#23817,#23818,#23819,
#23820,#23821,#23822,#23823,#23824,#23825,#23826,#23827,#23828,#23829,#23830,
#23831,#23832,#23833,#23834,#23835,#23836,#23837,#23838,#23839,#23840,#23841,
#23842,#23843,#23844,#23845,#23846,#23847,#23848,#23849,#23850,#23851,#23852,
#23853,#23854,#23855,#23856,#23857,#23858,#23859,#23860,#23861,#23862,#23863,
#23864,#23865,#23866,#23867,#23868,#23869,#23870,#23871,#23872,#23873,#23874,
#23875,#23876,#23877,#23878,#23879,#23880,#23881,#23882,#23883,#23884,#23885,
#23886,#23887,#23888,#23889,#23890,#23891,#23892,#23893,#23894,#23895,#23896,
#23897),(#23898,#23899,#23900,#23901,#23902,#23903,#23904,#23905,#23906,
#23907,#23908,#23909,#23910,#23911,#23912,#23913,#23914,#23915,#23916,#23917,
#23918,#23919,#23920,#23921,#23922,#23923,#23924,#23925,#23926,#23927,#23928,
#23929,#23930,#23931,#23932,#23933,#23934,#23935,#23936,#23937,#23938,#23939,
#23940,#23941,#23942,#23943,#23944,#23945,#23946,#23947,#23948,#23949,#23950,
#23951,#23952,#23953,#23954,#23955,#23956,#23957,#23958,#23959,#23960,#23961,
#23962,#23963,#23964,#23965,#23966,#23967,#23968,#23969,#23970,#23971,#23972,
#23973,#23974,#23975,#23976,#23977,#23978,#23979,#23980,#23981,#23982,#23983,
#23984,#23985,#23986,#23987,#23988,#23989,#23990,#23991,#23992,#23993,#23994,
#23995,#23996,#23997,#23998,#23999,#24000,#24001)),.UNSPECIFIED.,.F.,.F.,
 .F.,(4,4),(4,1,1,1,1,1,1,1,1,1,1,1,1,1,1,1,1,1,1,1,1,1,1,1,1,1,1,1,1,1,
1,1,1,1,1,1,1,1,1,1,1,1,1,1,1,1,1,1,1,1,1,1,1,1,1,1,1,1,1,1,1,1,1,1,1,1,
1,1,1,1,1,1,1,1,1,1,1,1,1,1,1,1,1,1,1,1,1,1,1,1,1,1,1,1,1,1,1,1,1,1,1,4),
(0.,0.0448889834294935),(14.3981410127769,15.3956695472135,16.3931980816501,
17.3907266160867,18.3882551505233,19.3857836849599,20.3833122193965,21.3808407538331,
22.3783692882697,23.3758978227063,24.3734263571429,25.3709548915795,26.3684834260161,
27.3660119604527,28.3635404948893,29.3610690293259,30.3585975637625,31.3561260981991,
32.3536546326357,33.3511831670723,34.3487117015089,35.3462402359455,36.3437687703821,
37.3412973048187,38.3388258392553,39.3363543736919,40.3338829081285,41.3314114425651,
42.3289399770017,43.3264685114383,44.3239970458749,45.3215255803115,46.3190541147481,
47.3165826491847,48.3141111836213,49.3116397180579,50.3091682524945,51.3066967869311,
52.3042253213677,53.3017538558043,54.2992823902409,55.2968109246775,56.2943394591141,
57.2918679935507,58.2893965279873,59.2869250624239,60.2844535968605,61.2819821312971,
62.2795106657337,63.2770392001703,64.2745677346069,65.2720962690435,66.2696248034801,
67.2671533379167,68.2646818723533,69.2622104067898,70.2597389412265,71.2572674756631,
72.2547960100997,73.2523245445363,74.2498530789728,75.2473816134095,76.244910147846,
77.2424386822827,78.2399672167193,79.2374957511558,80.2350242855924,81.232552820029,
82.2300813544657,83.2276098889023,84.2251384233388,85.2226669577754,86.220195492212,
87.2177240266486,88.2152525610852,89.2127810955218,90.2103096299584,91.207838164395,
92.2053666988316,93.2028952332682,94.2004237677048,95.1979523021414,96.195480836578,
97.1930093710146,98.1905379054512,99.1880664398878,100.185594974324,101.183123508761,
102.180652043198,103.178180577634,104.175709112071,105.173237646507,106.170766180944,
107.168294715381,108.165823249817,109.163351784254,110.16088031869,111.158408853127,
112.155937387564,113.153465922,114.150994456437,115.148522990873),
 .UNSPECIFIED.);
#303=B_SPLINE_SURFACE_WITH_KNOTS('',3,3,((#25336,#25337,#25338,#25339,#25340,
#25341,#25342,#25343,#25344,#25345,#25346,#25347,#25348,#25349,#25350,#25351,
#25352,#25353,#25354,#25355,#25356,#25357,#25358,#25359,#25360,#25361,#25362,
#25363,#25364,#25365,#25366,#25367,#25368,#25369,#25370,#25371,#25372,#25373,
#25374,#25375,#25376,#25377,#25378,#25379,#25380,#25381,#25382,#25383,#25384,
#25385,#25386,#25387,#25388,#25389,#25390,#25391,#25392,#25393,#25394,#25395,
#25396,#25397,#25398,#25399,#25400,#25401,#25402,#25403,#25404,#25405),
(#25406,#25407,#25408,#25409,#25410,#25411,#25412,#25413,#25414,#25415,
#25416,#25417,#25418,#25419,#25420,#25421,#25422,#25423,#25424,#25425,#25426,
#25427,#25428,#25429,#25430,#25431,#25432,#25433,#25434,#25435,#25436,#25437,
#25438,#25439,#25440,#25441,#25442,#25443,#25444,#25445,#25446,#25447,#25448,
#25449,#25450,#25451,#25452,#25453,#25454,#25455,#25456,#25457,#25458,#25459,
#25460,#25461,#25462,#25463,#25464,#25465,#25466,#25467,#25468,#25469,#25470,
#25471,#25472,#25473,#25474,#25475),(#25476,#25477,#25478,#25479,#25480,
#25481,#25482,#25483,#25484,#25485,#25486,#25487,#25488,#25489,#25490,#25491,
#25492,#25493,#25494,#25495,#25496,#25497,#25498,#25499,#25500,#25501,#25502,
#25503,#25504,#25505,#25506,#25507,#25508,#25509,#25510,#25511,#25512,#25513,
#25514,#25515,#25516,#25517,#25518,#25519,#25520,#25521,#25522,#25523,#25524,
#25525,#25526,#25527,#25528,#25529,#25530,#25531,#25532,#25533,#25534,#25535,
#25536,#25537,#25538,#25539,#25540,#25541,#25542,#25543,#25544,#25545),
(#25546,#25547,#25548,#25549,#25550,#25551,#25552,#25553,#25554,#25555,
#25556,#25557,#25558,#25559,#25560,#25561,#25562,#25563,#25564,#25565,#25566,
#25567,#25568,#25569,#25570,#25571,#25572,#25573,#25574,#25575,#25576,#25577,
#25578,#25579,#25580,#25581,#25582,#25583,#25584,#25585,#25586,#25587,#25588,
#25589,#25590,#25591,#25592,#25593,#25594,#25595,#25596,#25597,#25598,#25599,
#25600,#25601,#25602,#25603,#25604,#25605,#25606,#25607,#25608,#25609,#25610,
#25611,#25612,#25613,#25614,#25615)),.UNSPECIFIED.,.F.,.F.,.F.,(4,4),(4,
1,1,1,1,1,1,1,1,1,1,1,1,1,1,1,1,1,1,1,1,1,1,1,1,1,1,1,1,1,1,1,1,1,1,1,1,
1,1,1,1,1,1,1,1,1,1,1,1,1,1,1,1,1,1,1,1,1,1,1,1,1,1,1,1,1,1,4),(0.,0.0460148164544132),
(11.6154215191106,12.6127599630189,13.6100984069272,14.6074368508354,15.6047752947437,
16.602113738652,17.5994521825603,18.5967906264686,19.5941290703769,20.5914675142851,
21.5888059581934,22.5861444021017,23.58348284601,24.5808212899183,25.5781597338266,
26.5754981777348,27.5728366216431,28.5701750655514,29.5675135094597,30.564851953368,
31.5621903972762,32.5595288411845,33.5568672850928,34.5542057290011,35.5515441729094,
36.5488826168177,37.5462210607259,38.5435595046342,39.5408979485425,40.5382363924508,
41.5355748363591,42.5329132802674,43.5302517241756,44.5275901680839,45.5249286119922,
46.5222670559005,47.5196054998088,48.516943943717,49.5142823876253,50.5116208315336,
51.5089592754419,52.5062977193502,53.5036361632585,54.5009746071667,55.498313051075,
56.4956514949833,57.4929899388916,58.4903283827999,59.4876668267081,60.4850052706164,
61.4823437145247,62.479682158433,63.4770206023413,64.4743590462496,65.4716974901578,
66.4690359340661,67.4663743779744,68.4637128218827,69.461051265791,70.4583897096992,
71.4557281536075,72.4530665975158,73.4504050414241,74.4477434853324,75.4450819292407,
76.4424203731489,77.4397588170572,78.4370972609655),.UNSPECIFIED.);
#304=B_SPLINE_SURFACE_WITH_KNOTS('',3,3,((#25741,#25742,#25743,#25744,#25745,
#25746,#25747,#25748,#25749,#25750,#25751,#25752,#25753,#25754,#25755,#25756,
#25757,#25758,#25759,#25760,#25761,#25762,#25763,#25764,#25765,#25766,#25767,
#25768,#25769,#25770,#25771,#25772,#25773,#25774,#25775,#25776,#25777,#25778,
#25779,#25780,#25781,#25782,#25783,#25784,#25785,#25786,#25787,#25788,#25789,
#25790,#25791,#25792,#25793,#25794,#25795,#25796,#25797,#25798,#25799,#25800,
#25801,#25802,#25803,#25804,#25805,#25806,#25807,#25808,#25809,#25810,#25811,
#25812),(#25813,#25814,#25815,#25816,#25817,#25818,#25819,#25820,#25821,
#25822,#25823,#25824,#25825,#25826,#25827,#25828,#25829,#25830,#25831,#25832,
#25833,#25834,#25835,#25836,#25837,#25838,#25839,#25840,#25841,#25842,#25843,
#25844,#25845,#25846,#25847,#25848,#25849,#25850,#25851,#25852,#25853,#25854,
#25855,#25856,#25857,#25858,#25859,#25860,#25861,#25862,#25863,#25864,#25865,
#25866,#25867,#25868,#25869,#25870,#25871,#25872,#25873,#25874,#25875,#25876,
#25877,#25878,#25879,#25880,#25881,#25882,#25883,#25884),(#25885,#25886,
#25887,#25888,#25889,#25890,#25891,#25892,#25893,#25894,#25895,#25896,#25897,
#25898,#25899,#25900,#25901,#25902,#25903,#25904,#25905,#25906,#25907,#25908,
#25909,#25910,#25911,#25912,#25913,#25914,#25915,#25916,#25917,#25918,#25919,
#25920,#25921,#25922,#25923,#25924,#25925,#25926,#25927,#25928,#25929,#25930,
#25931,#25932,#25933,#25934,#25935,#25936,#25937,#25938,#25939,#25940,#25941,
#25942,#25943,#25944,#25945,#25946,#25947,#25948,#25949,#25950,#25951,#25952,
#25953,#25954,#25955,#25956),(#25957,#25958,#25959,#25960,#25961,#25962,
#25963,#25964,#25965,#25966,#25967,#25968,#25969,#25970,#25971,#25972,#25973,
#25974,#25975,#25976,#25977,#25978,#25979,#25980,#25981,#25982,#25983,#25984,
#25985,#25986,#25987,#25988,#25989,#25990,#25991,#25992,#25993,#25994,#25995,
#25996,#25997,#25998,#25999,#26000,#26001,#26002,#26003,#26004,#26005,#26006,
#26007,#26008,#26009,#26010,#26011,#26012,#26013,#26014,#26015,#26016,#26017,
#26018,#26019,#26020,#26021,#26022,#26023,#26024,#26025,#26026,#26027,#26028)),
 .UNSPECIFIED.,.F.,.F.,.F.,(4,4),(4,1,1,1,1,1,1,1,1,1,1,1,1,1,1,1,1,1,1,
1,1,1,1,1,1,1,1,1,1,1,1,1,1,1,1,1,1,1,1,1,1,1,1,1,1,1,1,1,1,1,1,1,1,1,1,
1,1,1,1,1,1,1,1,1,1,1,1,1,1,4),(0.,0.0460148164544132),(8.31058692273974,
9.30894657310399,10.3073062234682,11.3056658738325,12.3040255241967,13.302385174561,
14.3007448249252,15.2991044752895,16.2974641256537,17.295823776018,18.2941834263822,
19.2925430767465,20.2909027271107,21.289262377475,22.2876220278392,23.2859816782034,
24.2843413285677,25.2827009789319,26.2810606292962,27.2794202796604,28.2777799300247,
29.2761395803889,30.2744992307532,31.2728588811174,32.2712185314817,33.2695781818459,
34.2679378322102,35.2662974825744,36.2646571329387,37.2630167833029,38.2613764336672,
39.2597360840314,40.2580957343957,41.2564553847599,42.2548150351241,43.2531746854884,
44.2515343358526,45.2498939862169,46.2482536365811,47.2466132869454,48.2449729373096,
49.2433325876739,50.2416922380381,51.2400518884024,52.2384115387666,53.2367711891309,
54.2351308394951,55.2334904898594,56.2318501402236,57.2302097905879,58.2285694409521,
59.2269290913164,60.2252887416806,61.2236483920448,62.2220080424091,63.2203676927733,
64.2187273431376,65.2170869935018,66.2154466438661,67.2138062942303,68.2121659445946,
69.2105255949588,70.2088852453231,71.2072448956873,72.2056045460516,73.2039641964158,
74.2023238467801,75.2006834971443,76.1990431475085,77.1974027978728),
 .UNSPECIFIED.);
#305=B_SPLINE_SURFACE_WITH_KNOTS('',3,3,((#28103,#28104,#28105,#28106,#28107,
#28108,#28109,#28110,#28111,#28112,#28113,#28114,#28115,#28116,#28117,#28118,
#28119,#28120,#28121,#28122,#28123,#28124,#28125,#28126,#28127,#28128,#28129,
#28130,#28131,#28132,#28133,#28134,#28135,#28136,#28137,#28138,#28139,#28140,
#28141,#28142,#28143,#28144,#28145,#28146,#28147,#28148,#28149,#28150,#28151,
#28152,#28153,#28154,#28155,#28156,#28157,#28158,#28159,#28160,#28161,#28162,
#28163,#28164,#28165,#28166,#28167,#28168,#28169,#28170,#28171,#28172,#28173,
#28174,#28175,#28176,#28177,#28178,#28179,#28180,#28181,#28182,#28183,#28184,
#28185,#28186,#28187,#28188,#28189,#28190,#28191,#28192,#28193,#28194,#28195,
#28196,#28197,#28198,#28199,#28200,#28201,#28202,#28203,#28204,#28205,#28206,
#28207,#28208,#28209,#28210,#28211,#28212,#28213,#28214,#28215,#28216,#28217,
#28218,#28219,#28220,#28221,#28222,#28223,#28224,#28225,#28226,#28227,#28228,
#28229),(#28230,#28231,#28232,#28233,#28234,#28235,#28236,#28237,#28238,
#28239,#28240,#28241,#28242,#28243,#28244,#28245,#28246,#28247,#28248,#28249,
#28250,#28251,#28252,#28253,#28254,#28255,#28256,#28257,#28258,#28259,#28260,
#28261,#28262,#28263,#28264,#28265,#28266,#28267,#28268,#28269,#28270,#28271,
#28272,#28273,#28274,#28275,#28276,#28277,#28278,#28279,#28280,#28281,#28282,
#28283,#28284,#28285,#28286,#28287,#28288,#28289,#28290,#28291,#28292,#28293,
#28294,#28295,#28296,#28297,#28298,#28299,#28300,#28301,#28302,#28303,#28304,
#28305,#28306,#28307,#28308,#28309,#28310,#28311,#28312,#28313,#28314,#28315,
#28316,#28317,#28318,#28319,#28320,#28321,#28322,#28323,#28324,#28325,#28326,
#28327,#28328,#28329,#28330,#28331,#28332,#28333,#28334,#28335,#28336,#28337,
#28338,#28339,#28340,#28341,#28342,#28343,#28344,#28345,#28346,#28347,#28348,
#28349,#28350,#28351,#28352,#28353,#28354,#28355,#28356),(#28357,#28358,
#28359,#28360,#28361,#28362,#28363,#28364,#28365,#28366,#28367,#28368,#28369,
#28370,#28371,#28372,#28373,#28374,#28375,#28376,#28377,#28378,#28379,#28380,
#28381,#28382,#28383,#28384,#28385,#28386,#28387,#28388,#28389,#28390,#28391,
#28392,#28393,#28394,#28395,#28396,#28397,#28398,#28399,#28400,#28401,#28402,
#28403,#28404,#28405,#28406,#28407,#28408,#28409,#28410,#28411,#28412,#28413,
#28414,#28415,#28416,#28417,#28418,#28419,#28420,#28421,#28422,#28423,#28424,
#28425,#28426,#28427,#28428,#28429,#28430,#28431,#28432,#28433,#28434,#28435,
#28436,#28437,#28438,#28439,#28440,#28441,#28442,#28443,#28444,#28445,#28446,
#28447,#28448,#28449,#28450,#28451,#28452,#28453,#28454,#28455,#28456,#28457,
#28458,#28459,#28460,#28461,#28462,#28463,#28464,#28465,#28466,#28467,#28468,
#28469,#28470,#28471,#28472,#28473,#28474,#28475,#28476,#28477,#28478,#28479,
#28480,#28481,#28482,#28483),(#28484,#28485,#28486,#28487,#28488,#28489,
#28490,#28491,#28492,#28493,#28494,#28495,#28496,#28497,#28498,#28499,#28500,
#28501,#28502,#28503,#28504,#28505,#28506,#28507,#28508,#28509,#28510,#28511,
#28512,#28513,#28514,#28515,#28516,#28517,#28518,#28519,#28520,#28521,#28522,
#28523,#28524,#28525,#28526,#28527,#28528,#28529,#28530,#28531,#28532,#28533,
#28534,#28535,#28536,#28537,#28538,#28539,#28540,#28541,#28542,#28543,#28544,
#28545,#28546,#28547,#28548,#28549,#28550,#28551,#28552,#28553,#28554,#28555,
#28556,#28557,#28558,#28559,#28560,#28561,#28562,#28563,#28564,#28565,#28566,
#28567,#28568,#28569,#28570,#28571,#28572,#28573,#28574,#28575,#28576,#28577,
#28578,#28579,#28580,#28581,#28582,#28583,#28584,#28585,#28586,#28587,#28588,
#28589,#28590,#28591,#28592,#28593,#28594,#28595,#28596,#28597,#28598,#28599,
#28600,#28601,#28602,#28603,#28604,#28605,#28606,#28607,#28608,#28609,#28610)),
 .UNSPECIFIED.,.F.,.F.,.F.,(4,4),(4,1,1,1,1,1,1,1,1,1,1,1,1,1,1,1,1,1,1,
1,1,1,1,1,1,1,1,1,1,1,1,1,1,1,1,1,1,1,1,1,1,1,1,1,1,1,1,1,1,1,1,1,1,1,1,
1,1,1,1,1,1,1,1,1,1,1,1,1,1,1,1,1,1,1,1,1,1,1,1,1,1,1,1,1,1,1,1,1,1,1,1,
1,1,1,1,1,1,1,1,1,1,1,1,1,1,1,1,1,1,1,1,1,1,1,1,1,1,1,1,1,1,1,1,1,4),(0.,
0.0658467982010768),(11.6150328478182,12.609612944638,13.6041930414577,
14.5987731382775,15.5933532350972,16.5879333319169,17.5825134287367,18.5770935255564,
19.5716736223762,20.5662537191959,21.5608338160156,22.5554139128354,23.5499940096551,
24.5445741064749,25.5391542032946,26.5337343001143,27.5283143969341,28.5228944937538,
29.5174745905736,30.5120546873933,31.506634784213,32.5012148810328,33.4957949778525,
34.4903750746723,35.484955171492,36.4795352683117,37.4741153651315,38.4686954619512,
39.463275558771,40.4578556555907,41.4524357524104,42.4470158492302,43.4415959460499,
44.4361760428697,45.4307561396894,46.4253362365091,47.4199163333289,48.4144964301486,
49.4090765269684,50.4036566237881,51.3982367206078,52.3928168174276,53.3873969142473,
54.3819770110671,55.3765571078868,56.3711372047065,57.3657173015263,58.360297398346,
59.3548774951657,60.3494575919855,61.3440376888052,62.338617785625,63.3331978824447,
64.3277779792645,65.3223580760842,66.3169381729039,67.3115182697237,68.3060983665434,
69.3006784633631,70.2952585601829,71.2898386570026,72.2844187538224,73.2789988506421,
74.2735789474618,75.2681590442816,76.2627391411013,77.2573192379211,78.2518993347408,
79.2464794315605,80.2410595283803,81.2356396252,82.2302197220198,83.2247998188395,
84.2193799156592,85.213960012479,86.2085401092987,87.2031202061185,88.1977003029382,
89.1922803997579,90.1868604965777,91.1814405933974,92.1760206902171,93.1706007870369,
94.1651808838566,95.1597609806764,96.1543410774961,97.1489211743159,98.1435012711356,
99.1380813679553,100.132661464775,101.127241561595,102.121821658415,103.116401755234,
104.110981852054,105.105561948874,106.100142045694,107.094722142513,108.089302239333,
109.083882336153,110.078462432972,111.073042529792,112.067622626612,113.062202723432,
114.056782820251,115.051362917071,116.045943013891,117.040523110711,118.03510320753,
119.02968330435,120.02426340117,121.01884349799,122.013423594809,123.008003691629,
124.002583788449,124.997163885269,125.991743982088,126.986324078908,127.980904175728,
128.975484272548,129.970064369367,130.964644466187,131.959224563007,132.953804659826,
133.948384756646,134.942964853466),.UNSPECIFIED.);
#306=B_SPLINE_SURFACE_WITH_KNOTS('',3,3,((#28742,#28743,#28744,#28745,#28746,
#28747,#28748,#28749,#28750,#28751,#28752,#28753,#28754,#28755,#28756,#28757,
#28758,#28759,#28760,#28761,#28762,#28763,#28764,#28765,#28766,#28767,#28768,
#28769,#28770,#28771,#28772,#28773,#28774,#28775,#28776,#28777,#28778,#28779,
#28780,#28781,#28782,#28783,#28784,#28785,#28786,#28787,#28788,#28789,#28790,
#28791,#28792,#28793,#28794,#28795,#28796,#28797,#28798,#28799,#28800,#28801,
#28802,#28803,#28804,#28805,#28806,#28807,#28808,#28809,#28810,#28811,#28812,
#28813,#28814,#28815,#28816,#28817,#28818,#28819,#28820,#28821,#28822,#28823,
#28824,#28825,#28826,#28827,#28828,#28829,#28830,#28831,#28832,#28833,#28834,
#28835,#28836,#28837,#28838,#28839,#28840,#28841,#28842,#28843,#28844,#28845,
#28846,#28847,#28848,#28849,#28850,#28851,#28852,#28853,#28854,#28855,#28856,
#28857,#28858,#28859,#28860,#28861,#28862,#28863,#28864,#28865,#28866,#28867,
#28868,#28869,#28870),(#28871,#28872,#28873,#28874,#28875,#28876,#28877,
#28878,#28879,#28880,#28881,#28882,#28883,#28884,#28885,#28886,#28887,#28888,
#28889,#28890,#28891,#28892,#28893,#28894,#28895,#28896,#28897,#28898,#28899,
#28900,#28901,#28902,#28903,#28904,#28905,#28906,#28907,#28908,#28909,#28910,
#28911,#28912,#28913,#28914,#28915,#28916,#28917,#28918,#28919,#28920,#28921,
#28922,#28923,#28924,#28925,#28926,#28927,#28928,#28929,#28930,#28931,#28932,
#28933,#28934,#28935,#28936,#28937,#28938,#28939,#28940,#28941,#28942,#28943,
#28944,#28945,#28946,#28947,#28948,#28949,#28950,#28951,#28952,#28953,#28954,
#28955,#28956,#28957,#28958,#28959,#28960,#28961,#28962,#28963,#28964,#28965,
#28966,#28967,#28968,#28969,#28970,#28971,#28972,#28973,#28974,#28975,#28976,
#28977,#28978,#28979,#28980,#28981,#28982,#28983,#28984,#28985,#28986,#28987,
#28988,#28989,#28990,#28991,#28992,#28993,#28994,#28995,#28996,#28997,#28998,
#28999),(#29000,#29001,#29002,#29003,#29004,#29005,#29006,#29007,#29008,
#29009,#29010,#29011,#29012,#29013,#29014,#29015,#29016,#29017,#29018,#29019,
#29020,#29021,#29022,#29023,#29024,#29025,#29026,#29027,#29028,#29029,#29030,
#29031,#29032,#29033,#29034,#29035,#29036,#29037,#29038,#29039,#29040,#29041,
#29042,#29043,#29044,#29045,#29046,#29047,#29048,#29049,#29050,#29051,#29052,
#29053,#29054,#29055,#29056,#29057,#29058,#29059,#29060,#29061,#29062,#29063,
#29064,#29065,#29066,#29067,#29068,#29069,#29070,#29071,#29072,#29073,#29074,
#29075,#29076,#29077,#29078,#29079,#29080,#29081,#29082,#29083,#29084,#29085,
#29086,#29087,#29088,#29089,#29090,#29091,#29092,#29093,#29094,#29095,#29096,
#29097,#29098,#29099,#29100,#29101,#29102,#29103,#29104,#29105,#29106,#29107,
#29108,#29109,#29110,#29111,#29112,#29113,#29114,#29115,#29116,#29117,#29118,
#29119,#29120,#29121,#29122,#29123,#29124,#29125,#29126,#29127,#29128),
(#29129,#29130,#29131,#29132,#29133,#29134,#29135,#29136,#29137,#29138,
#29139,#29140,#29141,#29142,#29143,#29144,#29145,#29146,#29147,#29148,#29149,
#29150,#29151,#29152,#29153,#29154,#29155,#29156,#29157,#29158,#29159,#29160,
#29161,#29162,#29163,#29164,#29165,#29166,#29167,#29168,#29169,#29170,#29171,
#29172,#29173,#29174,#29175,#29176,#29177,#29178,#29179,#29180,#29181,#29182,
#29183,#29184,#29185,#29186,#29187,#29188,#29189,#29190,#29191,#29192,#29193,
#29194,#29195,#29196,#29197,#29198,#29199,#29200,#29201,#29202,#29203,#29204,
#29205,#29206,#29207,#29208,#29209,#29210,#29211,#29212,#29213,#29214,#29215,
#29216,#29217,#29218,#29219,#29220,#29221,#29222,#29223,#29224,#29225,#29226,
#29227,#29228,#29229,#29230,#29231,#29232,#29233,#29234,#29235,#29236,#29237,
#29238,#29239,#29240,#29241,#29242,#29243,#29244,#29245,#29246,#29247,#29248,
#29249,#29250,#29251,#29252,#29253,#29254,#29255,#29256,#29257)),
 .UNSPECIFIED.,.F.,.F.,.F.,(4,4),(4,1,1,1,1,1,1,1,1,1,1,1,1,1,1,1,1,1,1,
1,1,1,1,1,1,1,1,1,1,1,1,1,1,1,1,1,1,1,1,1,1,1,1,1,1,1,1,1,1,1,1,1,1,1,1,
1,1,1,1,1,1,1,1,1,1,1,1,1,1,1,1,1,1,1,1,1,1,1,1,1,1,1,1,1,1,1,1,1,1,1,1,
1,1,1,1,1,1,1,1,1,1,1,1,1,1,1,1,1,1,1,1,1,1,1,1,1,1,1,1,1,1,1,1,1,1,1,4),
(0.,0.0658467982010768),(8.30747755240104,9.3026884268499,10.2978993012988,
11.2931101757476,12.2883210501965,13.2835319246454,14.2787427990942,15.2739536735431,
16.2691645479919,17.2643754224408,18.2595862968897,19.2547971713385,20.2500080457874,
21.2452189202363,22.2404297946851,23.235640669134,24.2308515435829,25.2260624180317,
26.2212732924806,27.2164841669295,28.2116950413783,29.2069059158272,30.202116790276,
31.1973276647249,32.1925385391738,33.1877494136226,34.1829602880715,35.1781711625204,
36.1733820369692,37.1685929114181,38.163803785867,39.1590146603158,40.1542255347647,
41.1494364092135,42.1446472836624,43.1398581581113,44.1350690325601,45.130279907009,
46.1254907814579,47.1207016559067,48.1159125303556,49.1111234048045,50.1063342792533,
51.1015451537022,52.096756028151,53.0919669025999,54.0871777770488,55.0823886514976,
56.0775995259465,57.0728104003954,58.0680212748442,59.0632321492931,60.058443023742,
61.0536538981908,62.0488647726397,63.0440756470886,64.0392865215374,65.0344973959863,
66.0297082704352,67.024919144884,68.0201300193329,69.0153408937817,70.0105517682306,
71.0057626426795,72.0009735171283,72.9961843915772,73.9913952660261,74.9866061404749,
75.9818170149238,76.9770278893726,77.9722387638215,78.9674496382704,79.9626605127192,
80.9578713871681,81.953082261617,82.9482931360658,83.9435040105147,84.9387148849636,
85.9339257594124,86.9291366338613,87.9243475083101,88.919558382759,89.9147692572079,
90.9099801316567,91.9051910061056,92.9004018805545,93.8956127550033,94.8908236294522,
95.8860345039011,96.8812453783499,97.8764562527988,98.8716671272477,99.8668780016965,
100.862088876145,101.857299750594,102.852510625043,103.847721499492,104.842932373941,
105.83814324839,106.833354122839,107.828564997287,108.823775871736,109.818986746185,
110.814197620634,111.809408495083,112.804619369532,113.799830243981,114.795041118429,
115.790251992878,116.785462867327,117.780673741776,118.775884616225,119.771095490674,
120.766306365123,121.761517239572,122.75672811402,123.751938988469,124.747149862918,
125.742360737367,126.737571611816,127.732782486265,128.727993360714,129.723204235162,
130.718415109611,131.71362598406,132.708836858509,133.704047732958),
 .UNSPECIFIED.);
#307=B_SPLINE_SURFACE_WITH_KNOTS('',3,3,((#30530,#30531,#30532,#30533,#30534,
#30535,#30536,#30537,#30538,#30539,#30540,#30541,#30542,#30543,#30544,#30545,
#30546,#30547,#30548,#30549,#30550,#30551,#30552,#30553,#30554,#30555,#30556,
#30557,#30558,#30559,#30560,#30561,#30562,#30563,#30564,#30565,#30566,#30567,
#30568,#30569,#30570,#30571,#30572,#30573,#30574,#30575,#30576,#30577,#30578,
#30579,#30580,#30581,#30582,#30583,#30584,#30585,#30586,#30587,#30588,#30589,
#30590,#30591,#30592,#30593,#30594,#30595,#30596,#30597,#30598,#30599,#30600,
#30601,#30602,#30603,#30604,#30605,#30606),(#30607,#30608,#30609,#30610,
#30611,#30612,#30613,#30614,#30615,#30616,#30617,#30618,#30619,#30620,#30621,
#30622,#30623,#30624,#30625,#30626,#30627,#30628,#30629,#30630,#30631,#30632,
#30633,#30634,#30635,#30636,#30637,#30638,#30639,#30640,#30641,#30642,#30643,
#30644,#30645,#30646,#30647,#30648,#30649,#30650,#30651,#30652,#30653,#30654,
#30655,#30656,#30657,#30658,#30659,#30660,#30661,#30662,#30663,#30664,#30665,
#30666,#30667,#30668,#30669,#30670,#30671,#30672,#30673,#30674,#30675,#30676,
#30677,#30678,#30679,#30680,#30681,#30682,#30683),(#30684,#30685,#30686,
#30687,#30688,#30689,#30690,#30691,#30692,#30693,#30694,#30695,#30696,#30697,
#30698,#30699,#30700,#30701,#30702,#30703,#30704,#30705,#30706,#30707,#30708,
#30709,#30710,#30711,#30712,#30713,#30714,#30715,#30716,#30717,#30718,#30719,
#30720,#30721,#30722,#30723,#30724,#30725,#30726,#30727,#30728,#30729,#30730,
#30731,#30732,#30733,#30734,#30735,#30736,#30737,#30738,#30739,#30740,#30741,
#30742,#30743,#30744,#30745,#30746,#30747,#30748,#30749,#30750,#30751,#30752,
#30753,#30754,#30755,#30756,#30757,#30758,#30759,#30760),(#30761,#30762,
#30763,#30764,#30765,#30766,#30767,#30768,#30769,#30770,#30771,#30772,#30773,
#30774,#30775,#30776,#30777,#30778,#30779,#30780,#30781,#30782,#30783,#30784,
#30785,#30786,#30787,#30788,#30789,#30790,#30791,#30792,#30793,#30794,#30795,
#30796,#30797,#30798,#30799,#30800,#30801,#30802,#30803,#30804,#30805,#30806,
#30807,#30808,#30809,#30810,#30811,#30812,#30813,#30814,#30815,#30816,#30817,
#30818,#30819,#30820,#30821,#30822,#30823,#30824,#30825,#30826,#30827,#30828,
#30829,#30830,#30831,#30832,#30833,#30834,#30835,#30836,#30837)),
 .UNSPECIFIED.,.F.,.F.,.F.,(4,4),(4,1,1,1,1,1,1,1,1,1,1,1,1,1,1,1,1,1,1,
1,1,1,1,1,1,1,1,1,1,1,1,1,1,1,1,1,1,1,1,1,1,1,1,1,1,1,1,1,1,1,1,1,1,1,1,
1,1,1,1,1,1,1,1,1,1,1,1,1,1,1,1,1,1,1,4),(0.,0.0658467982010768),(11.6150328478182,
12.6023632471184,13.5896936464185,14.5770240457187,15.5643544450188,16.551684844319,
17.5390152436191,18.5263456429193,19.5136760422194,20.5010064415196,21.4883368408197,
22.4756672401199,23.46299763942,24.4503280387202,25.4376584380203,26.4249888373205,
27.4123192366206,28.3996496359208,29.3869800352209,30.3743104345211,31.3616408338212,
32.3489712331214,33.3363016324215,34.3236320317217,35.3109624310218,36.298292830322,
37.2856232296221,38.2729536289223,39.2602840282224,40.2476144275226,41.2349448268227,
42.2222752261229,43.209605625423,44.1969360247232,45.1842664240233,46.1715968233235,
47.1589272226236,48.1462576219238,49.1335880212239,50.1209184205241,51.1082488198242,
52.0955792191244,53.0829096184245,54.0702400177247,55.0575704170248,56.0449008163249,
57.0322312156251,58.0195616149252,59.0068920142254,59.9942224135255,60.9815528128257,
61.9688832121258,62.956213611426,63.9435440107261,64.9308744100263,65.9182048093264,
66.9055352086266,67.8928656079267,68.8801960072269,69.867526406527,70.8548568058272,
71.8421872051273,72.8295176044275,73.8168480037276,74.8041784030278,75.7915088023279,
76.7788392016281,77.7661696009282,78.7535000002284,79.7408303995285,80.7281607988287,
81.7154911981288,82.702821597429,83.6901519967291,84.6774823960293),
 .UNSPECIFIED.);
#308=B_SPLINE_SURFACE_WITH_KNOTS('',3,3,((#30966,#30967,#30968,#30969,#30970,
#30971,#30972,#30973,#30974,#30975,#30976,#30977,#30978,#30979,#30980,#30981,
#30982,#30983,#30984,#30985,#30986,#30987,#30988,#30989,#30990,#30991,#30992,
#30993,#30994,#30995,#30996,#30997,#30998,#30999,#31000,#31001,#31002,#31003,
#31004,#31005,#31006,#31007,#31008,#31009,#31010,#31011,#31012,#31013,#31014,
#31015,#31016,#31017,#31018,#31019,#31020,#31021,#31022,#31023,#31024,#31025,
#31026,#31027,#31028,#31029,#31030,#31031,#31032,#31033,#31034,#31035,#31036,
#31037,#31038,#31039,#31040,#31041,#31042,#31043,#31044),(#31045,#31046,
#31047,#31048,#31049,#31050,#31051,#31052,#31053,#31054,#31055,#31056,#31057,
#31058,#31059,#31060,#31061,#31062,#31063,#31064,#31065,#31066,#31067,#31068,
#31069,#31070,#31071,#31072,#31073,#31074,#31075,#31076,#31077,#31078,#31079,
#31080,#31081,#31082,#31083,#31084,#31085,#31086,#31087,#31088,#31089,#31090,
#31091,#31092,#31093,#31094,#31095,#31096,#31097,#31098,#31099,#31100,#31101,
#31102,#31103,#31104,#31105,#31106,#31107,#31108,#31109,#31110,#31111,#31112,
#31113,#31114,#31115,#31116,#31117,#31118,#31119,#31120,#31121,#31122,#31123),
(#31124,#31125,#31126,#31127,#31128,#31129,#31130,#31131,#31132,#31133,
#31134,#31135,#31136,#31137,#31138,#31139,#31140,#31141,#31142,#31143,#31144,
#31145,#31146,#31147,#31148,#31149,#31150,#31151,#31152,#31153,#31154,#31155,
#31156,#31157,#31158,#31159,#31160,#31161,#31162,#31163,#31164,#31165,#31166,
#31167,#31168,#31169,#31170,#31171,#31172,#31173,#31174,#31175,#31176,#31177,
#31178,#31179,#31180,#31181,#31182,#31183,#31184,#31185,#31186,#31187,#31188,
#31189,#31190,#31191,#31192,#31193,#31194,#31195,#31196,#31197,#31198,#31199,
#31200,#31201,#31202),(#31203,#31204,#31205,#31206,#31207,#31208,#31209,
#31210,#31211,#31212,#31213,#31214,#31215,#31216,#31217,#31218,#31219,#31220,
#31221,#31222,#31223,#31224,#31225,#31226,#31227,#31228,#31229,#31230,#31231,
#31232,#31233,#31234,#31235,#31236,#31237,#31238,#31239,#31240,#31241,#31242,
#31243,#31244,#31245,#31246,#31247,#31248,#31249,#31250,#31251,#31252,#31253,
#31254,#31255,#31256,#31257,#31258,#31259,#31260,#31261,#31262,#31263,#31264,
#31265,#31266,#31267,#31268,#31269,#31270,#31271,#31272,#31273,#31274,#31275,
#31276,#31277,#31278,#31279,#31280,#31281)),.UNSPECIFIED.,.F.,.F.,.F.,(4,
4),(4,1,1,1,1,1,1,1,1,1,1,1,1,1,1,1,1,1,1,1,1,1,1,1,1,1,1,1,1,1,1,1,1,1,
1,1,1,1,1,1,1,1,1,1,1,1,1,1,1,1,1,1,1,1,1,1,1,1,1,1,1,1,1,1,1,1,1,1,1,1,
1,1,1,1,1,1,4),(0.,0.0658467982010768),(8.30747755240104,9.2960444961263,
10.2846114398516,11.2731783835768,12.2617453273021,13.2503122710274,14.2388792147526,
15.2274461584779,16.2160131022032,17.2045800459284,18.1931469896537,19.181713933379,
20.1702808771042,21.1588478208295,22.1474147645547,23.13598170828,24.1245486520053,
25.1131155957305,26.1016825394558,27.0902494831811,28.0788164269063,29.0673833706316,
30.0559503143569,31.0445172580821,32.0330842018074,33.0216511455327,34.0102180892579,
34.9987850329832,35.9873519767085,36.9759189204337,37.964485864159,38.9530528078842,
39.9416197516095,40.9301866953348,41.91875363906,42.9073205827853,43.8958875265106,
44.8844544702358,45.8730214139611,46.8615883576864,47.8501553014116,48.8387222451369,
49.8272891888622,50.8158561325874,51.8044230763127,52.792990020038,53.7815569637632,
54.7701239074885,55.7586908512138,56.747257794939,57.7358247386643,58.7243916823895,
59.7129586261148,60.7015255698401,61.6900925135653,62.6786594572906,63.6672264010159,
64.6557933447411,65.6443602884664,66.6329272321917,67.6214941759169,68.6100611196422,
69.5986280633675,70.5871950070927,71.575761950818,72.5643288945433,73.5528958382685,
74.5414627819938,75.530029725719,76.5185966694443,77.5071636131696,78.4957305568948,
79.4842975006201,80.4728644443454,81.4614313880706,82.4499983317959,83.4385652755212),
 .UNSPECIFIED.);
#309=B_SPLINE_SURFACE_WITH_KNOTS('',3,3,((#31802,#31803,#31804,#31805,#31806,
#31807,#31808,#31809,#31810,#31811,#31812,#31813,#31814,#31815,#31816,#31817,
#31818,#31819,#31820,#31821,#31822,#31823,#31824,#31825,#31826,#31827,#31828,
#31829,#31830,#31831,#31832,#31833,#31834,#31835,#31836,#31837,#31838),
(#31839,#31840,#31841,#31842,#31843,#31844,#31845,#31846,#31847,#31848,
#31849,#31850,#31851,#31852,#31853,#31854,#31855,#31856,#31857,#31858,#31859,
#31860,#31861,#31862,#31863,#31864,#31865,#31866,#31867,#31868,#31869,#31870,
#31871,#31872,#31873,#31874,#31875),(#31876,#31877,#31878,#31879,#31880,
#31881,#31882,#31883,#31884,#31885,#31886,#31887,#31888,#31889,#31890,#31891,
#31892,#31893,#31894,#31895,#31896,#31897,#31898,#31899,#31900,#31901,#31902,
#31903,#31904,#31905,#31906,#31907,#31908,#31909,#31910,#31911,#31912),
(#31913,#31914,#31915,#31916,#31917,#31918,#31919,#31920,#31921,#31922,
#31923,#31924,#31925,#31926,#31927,#31928,#31929,#31930,#31931,#31932,#31933,
#31934,#31935,#31936,#31937,#31938,#31939,#31940,#31941,#31942,#31943,#31944,
#31945,#31946,#31947,#31948,#31949)),.UNSPECIFIED.,.F.,.F.,.F.,(4,4),(4,
1,1,1,1,1,1,1,1,1,1,1,1,1,1,1,1,1,1,1,1,1,1,1,1,1,1,1,1,1,1,1,1,1,4),(0.,
0.0642013499338864),(11.8589888623078,12.8423086102174,13.825628358127,
14.8089481060366,15.7922678539462,16.7755876018558,17.7589073497654,18.742227097675,
19.7255468455846,20.7088665934942,21.6921863414038,22.6755060893134,23.658825837223,
24.6421455851326,25.6254653330422,26.6087850809518,27.5921048288614,28.575424576771,
29.5587443246806,30.5420640725902,31.5253838204998,32.5087035684094,33.492023316319,
34.4753430642286,35.4586628121382,36.4419825600478,37.4253023079574,38.408622055867,
39.3919418037766,40.3752615516862,41.3585812995958,42.3419010475054,43.325220795415,
44.3085405433246,45.2918602912342),.UNSPECIFIED.);
#310=B_SPLINE_SURFACE_WITH_KNOTS('',3,3,((#32157,#32158,#32159,#32160,#32161,
#32162,#32163,#32164,#32165,#32166,#32167,#32168,#32169,#32170,#32171,#32172,
#32173,#32174,#32175,#32176,#32177,#32178,#32179,#32180,#32181,#32182,#32183,
#32184,#32185,#32186,#32187,#32188,#32189,#32190,#32191,#32192,#32193),
(#32194,#32195,#32196,#32197,#32198,#32199,#32200,#32201,#32202,#32203,
#32204,#32205,#32206,#32207,#32208,#32209,#32210,#32211,#32212,#32213,#32214,
#32215,#32216,#32217,#32218,#32219,#32220,#32221,#32222,#32223,#32224,#32225,
#32226,#32227,#32228,#32229,#32230),(#32231,#32232,#32233,#32234,#32235,
#32236,#32237,#32238,#32239,#32240,#32241,#32242,#32243,#32244,#32245,#32246,
#32247,#32248,#32249,#32250,#32251,#32252,#32253,#32254,#32255,#32256,#32257,
#32258,#32259,#32260,#32261,#32262,#32263,#32264,#32265,#32266,#32267),
(#32268,#32269,#32270,#32271,#32272,#32273,#32274,#32275,#32276,#32277,
#32278,#32279,#32280,#32281,#32282,#32283,#32284,#32285,#32286,#32287,#32288,
#32289,#32290,#32291,#32292,#32293,#32294,#32295,#32296,#32297,#32298,#32299,
#32300,#32301,#32302,#32303,#32304)),.UNSPECIFIED.,.F.,.F.,.F.,(4,4),(4,
1,1,1,1,1,1,1,1,1,1,1,1,1,1,1,1,1,1,1,1,1,1,1,1,1,1,1,1,1,1,1,1,1,4),(0.,
0.0642013499338863),(14.3984001269719,15.3817198748815,16.3650396227911,
17.3483593707007,18.3316791186103,19.3149988665199,20.2983186144295,21.2816383623391,
22.2649581102487,23.2482778581583,24.2315976060679,25.2149173539775,26.1982371018871,
27.1815568497966,28.1648765977063,29.1481963456159,30.1315160935254,31.114835841435,
32.0981555893446,33.0814753372542,34.0647950851639,35.0481148330734,36.031434580983,
37.0147543288926,37.9980740768022,38.9813938247118,39.9647135726214,40.948033320531,
41.9313530684406,42.9146728163502,43.8979925642598,44.8813123121694,45.864632060079,
46.8479518079886,47.8312715558982),.UNSPECIFIED.);
#311=PLANE('',#9054);
#312=PLANE('',#9057);
#313=PLANE('',#9060);
#314=PLANE('',#9063);
#315=PLANE('',#9066);
#316=PLANE('',#9067);
#317=PLANE('',#9068);
#318=PLANE('',#9069);
#319=PLANE('',#9070);
#320=PLANE('',#9071);
#321=PLANE('',#9072);
#322=PLANE('',#9073);
#323=PLANE('',#9074);
#324=PLANE('',#9075);
#325=PLANE('',#9076);
#326=PLANE('',#9077);
#327=PLANE('',#9078);
#328=PLANE('',#9079);
#329=PLANE('',#9096);
#330=PLANE('',#9097);
#331=PLANE('',#9098);
#332=PLANE('',#9099);
#333=PLANE('',#9100);
#334=PLANE('',#9101);
#335=PLANE('',#9103);
#336=PLANE('',#9104);
#337=PLANE('',#9105);
#338=PLANE('',#9106);
#339=PLANE('',#9107);
#340=PLANE('',#9108);
#341=PLANE('',#9109);
#342=PLANE('',#9110);
#343=PLANE('',#9111);
#344=PLANE('',#9112);
#345=PLANE('',#9150);
#346=PLANE('',#9153);
#347=PLANE('',#9154);
#348=PLANE('',#9155);
#349=PLANE('',#9156);
#350=PLANE('',#9157);
#351=PLANE('',#9158);
#352=PLANE('',#9162);
#353=PLANE('',#9164);
#354=PLANE('',#9168);
#355=PLANE('',#9169);
#356=PLANE('',#9170);
#357=PLANE('',#9171);
#358=PLANE('',#9172);
#359=PLANE('',#9173);
#360=PLANE('',#9174);
#361=PLANE('',#9175);
#362=PLANE('',#9180);
#363=PLANE('',#9182);
#364=PLANE('',#9184);
#365=PLANE('',#9185);
#366=PLANE('',#9186);
#367=PLANE('',#9187);
#368=PLANE('',#9188);
#369=PLANE('',#9189);
#370=PLANE('',#9190);
#371=PLANE('',#9191);
#372=PLANE('',#9192);
#373=PLANE('',#9193);
#374=PLANE('',#9194);
#375=PLANE('',#9195);
#376=PLANE('',#9203);
#377=PLANE('',#9204);
#378=PLANE('',#9206);
#379=PLANE('',#9207);
#380=PLANE('',#9208);
#381=PLANE('',#9215);
#382=PLANE('',#9223);
#383=PLANE('',#9224);
#384=PLANE('',#9254);
#385=PLANE('',#9255);
#386=PLANE('',#9256);
#387=PLANE('',#9257);
#388=PLANE('',#9258);
#389=PLANE('',#9259);
#390=PLANE('',#9260);
#391=PLANE('',#9261);
#392=PLANE('',#9265);
#393=PLANE('',#9266);
#394=PLANE('',#9268);
#395=PLANE('',#9269);
#396=PLANE('',#9282);
#397=PLANE('',#9283);
#398=PLANE('',#9290);
#399=PLANE('',#9291);
#400=PLANE('',#9292);
#401=PLANE('',#9293);
#402=PLANE('',#9298);
#403=PLANE('',#9300);
#404=PLANE('',#9304);
#405=PLANE('',#9309);
#406=PLANE('',#9311);
#407=PLANE('',#9313);
#408=PLANE('',#9314);
#409=PLANE('',#9315);
#410=PLANE('',#9322);
#411=PLANE('',#9324);
#412=PLANE('',#9325);
#413=PLANE('',#9326);
#414=PLANE('',#9329);
#415=PLANE('',#9334);
#416=PLANE('',#9341);
#417=PLANE('',#9342);
#418=PLANE('',#9343);
#419=PLANE('',#9344);
#420=PLANE('',#9352);
#421=PLANE('',#9353);
#422=PLANE('',#9401);
#423=PLANE('',#9402);
#424=PLANE('',#9403);
#425=PLANE('',#9404);
#426=PLANE('',#9405);
#427=PLANE('',#9406);
#428=PLANE('',#9407);
#429=PLANE('',#9408);
#430=PLANE('',#9412);
#431=PLANE('',#9413);
#432=PLANE('',#9445);
#433=PLANE('',#9446);
#434=PLANE('',#9447);
#435=PLANE('',#9448);
#436=PLANE('',#9449);
#437=PLANE('',#9450);
#438=PLANE('',#9451);
#439=PLANE('',#9452);
#440=PLANE('',#9456);
#441=PLANE('',#9457);
#442=PLANE('',#9465);
#443=PLANE('',#9466);
#444=PLANE('',#9483);
#445=PLANE('',#9485);
#446=PLANE('',#9486);
#447=PLANE('',#9487);
#448=PLANE('',#9488);
#449=PLANE('',#9489);
#450=PLANE('',#9490);
#451=PLANE('',#9491);
#452=FACE_OUTER_BOUND('',#927,.T.);
#453=FACE_OUTER_BOUND('',#928,.T.);
#454=FACE_OUTER_BOUND('',#929,.T.);
#455=FACE_OUTER_BOUND('',#930,.T.);
#456=FACE_OUTER_BOUND('',#931,.T.);
#457=FACE_OUTER_BOUND('',#932,.T.);
#458=FACE_OUTER_BOUND('',#933,.T.);
#459=FACE_OUTER_BOUND('',#934,.T.);
#460=FACE_OUTER_BOUND('',#935,.T.);
#461=FACE_OUTER_BOUND('',#936,.T.);
#462=FACE_OUTER_BOUND('',#937,.T.);
#463=FACE_OUTER_BOUND('',#938,.T.);
#464=FACE_OUTER_BOUND('',#939,.T.);
#465=FACE_OUTER_BOUND('',#940,.T.);
#466=FACE_OUTER_BOUND('',#941,.T.);
#467=FACE_OUTER_BOUND('',#942,.T.);
#468=FACE_OUTER_BOUND('',#943,.T.);
#469=FACE_OUTER_BOUND('',#944,.T.);
#470=FACE_OUTER_BOUND('',#945,.T.);
#471=FACE_OUTER_BOUND('',#946,.T.);
#472=FACE_OUTER_BOUND('',#947,.T.);
#473=FACE_OUTER_BOUND('',#948,.T.);
#474=FACE_OUTER_BOUND('',#949,.T.);
#475=FACE_OUTER_BOUND('',#950,.T.);
#476=FACE_OUTER_BOUND('',#951,.T.);
#477=FACE_OUTER_BOUND('',#952,.T.);
#478=FACE_OUTER_BOUND('',#953,.T.);
#479=FACE_OUTER_BOUND('',#954,.T.);
#480=FACE_OUTER_BOUND('',#955,.T.);
#481=FACE_OUTER_BOUND('',#956,.T.);
#482=FACE_OUTER_BOUND('',#957,.T.);
#483=FACE_OUTER_BOUND('',#958,.T.);
#484=FACE_OUTER_BOUND('',#959,.T.);
#485=FACE_OUTER_BOUND('',#960,.T.);
#486=FACE_OUTER_BOUND('',#961,.T.);
#487=FACE_OUTER_BOUND('',#962,.T.);
#488=FACE_OUTER_BOUND('',#963,.T.);
#489=FACE_OUTER_BOUND('',#964,.T.);
#490=FACE_OUTER_BOUND('',#965,.T.);
#491=FACE_OUTER_BOUND('',#966,.T.);
#492=FACE_OUTER_BOUND('',#967,.T.);
#493=FACE_OUTER_BOUND('',#968,.T.);
#494=FACE_OUTER_BOUND('',#969,.T.);
#495=FACE_OUTER_BOUND('',#970,.T.);
#496=FACE_OUTER_BOUND('',#971,.T.);
#497=FACE_OUTER_BOUND('',#972,.T.);
#498=FACE_OUTER_BOUND('',#973,.T.);
#499=FACE_OUTER_BOUND('',#974,.T.);
#500=FACE_OUTER_BOUND('',#975,.T.);
#501=FACE_OUTER_BOUND('',#976,.T.);
#502=FACE_OUTER_BOUND('',#977,.T.);
#503=FACE_OUTER_BOUND('',#978,.T.);
#504=FACE_OUTER_BOUND('',#979,.T.);
#505=FACE_OUTER_BOUND('',#980,.T.);
#506=FACE_OUTER_BOUND('',#981,.T.);
#507=FACE_OUTER_BOUND('',#982,.T.);
#508=FACE_OUTER_BOUND('',#983,.T.);
#509=FACE_OUTER_BOUND('',#984,.T.);
#510=FACE_OUTER_BOUND('',#985,.T.);
#511=FACE_OUTER_BOUND('',#986,.T.);
#512=FACE_OUTER_BOUND('',#987,.T.);
#513=FACE_OUTER_BOUND('',#988,.T.);
#514=FACE_OUTER_BOUND('',#989,.T.);
#515=FACE_OUTER_BOUND('',#990,.T.);
#516=FACE_OUTER_BOUND('',#991,.T.);
#517=FACE_OUTER_BOUND('',#992,.T.);
#518=FACE_OUTER_BOUND('',#993,.T.);
#519=FACE_OUTER_BOUND('',#994,.T.);
#520=FACE_OUTER_BOUND('',#995,.T.);
#521=FACE_OUTER_BOUND('',#996,.T.);
#522=FACE_OUTER_BOUND('',#997,.T.);
#523=FACE_OUTER_BOUND('',#998,.T.);
#524=FACE_OUTER_BOUND('',#999,.T.);
#525=FACE_OUTER_BOUND('',#1000,.T.);
#526=FACE_OUTER_BOUND('',#1001,.T.);
#527=FACE_OUTER_BOUND('',#1002,.T.);
#528=FACE_OUTER_BOUND('',#1003,.T.);
#529=FACE_OUTER_BOUND('',#1004,.T.);
#530=FACE_OUTER_BOUND('',#1005,.T.);
#531=FACE_OUTER_BOUND('',#1006,.T.);
#532=FACE_OUTER_BOUND('',#1007,.T.);
#533=FACE_OUTER_BOUND('',#1008,.T.);
#534=FACE_OUTER_BOUND('',#1009,.T.);
#535=FACE_OUTER_BOUND('',#1010,.T.);
#536=FACE_OUTER_BOUND('',#1011,.T.);
#537=FACE_OUTER_BOUND('',#1012,.T.);
#538=FACE_OUTER_BOUND('',#1013,.T.);
#539=FACE_OUTER_BOUND('',#1014,.T.);
#540=FACE_OUTER_BOUND('',#1015,.T.);
#541=FACE_OUTER_BOUND('',#1016,.T.);
#542=FACE_OUTER_BOUND('',#1017,.T.);
#543=FACE_OUTER_BOUND('',#1018,.T.);
#544=FACE_OUTER_BOUND('',#1019,.T.);
#545=FACE_OUTER_BOUND('',#1020,.T.);
#546=FACE_OUTER_BOUND('',#1021,.T.);
#547=FACE_OUTER_BOUND('',#1022,.T.);
#548=FACE_OUTER_BOUND('',#1023,.T.);
#549=FACE_OUTER_BOUND('',#1024,.T.);
#550=FACE_OUTER_BOUND('',#1025,.T.);
#551=FACE_OUTER_BOUND('',#1026,.T.);
#552=FACE_OUTER_BOUND('',#1027,.T.);
#553=FACE_OUTER_BOUND('',#1028,.T.);
#554=FACE_OUTER_BOUND('',#1029,.T.);
#555=FACE_OUTER_BOUND('',#1030,.T.);
#556=FACE_OUTER_BOUND('',#1031,.T.);
#557=FACE_OUTER_BOUND('',#1032,.T.);
#558=FACE_OUTER_BOUND('',#1033,.T.);
#559=FACE_OUTER_BOUND('',#1034,.T.);
#560=FACE_OUTER_BOUND('',#1035,.T.);
#561=FACE_OUTER_BOUND('',#1036,.T.);
#562=FACE_OUTER_BOUND('',#1037,.T.);
#563=FACE_OUTER_BOUND('',#1038,.T.);
#564=FACE_OUTER_BOUND('',#1039,.T.);
#565=FACE_OUTER_BOUND('',#1040,.T.);
#566=FACE_OUTER_BOUND('',#1041,.T.);
#567=FACE_OUTER_BOUND('',#1042,.T.);
#568=FACE_OUTER_BOUND('',#1043,.T.);
#569=FACE_OUTER_BOUND('',#1044,.T.);
#570=FACE_OUTER_BOUND('',#1045,.T.);
#571=FACE_OUTER_BOUND('',#1046,.T.);
#572=FACE_OUTER_BOUND('',#1047,.T.);
#573=FACE_OUTER_BOUND('',#1048,.T.);
#574=FACE_OUTER_BOUND('',#1049,.T.);
#575=FACE_OUTER_BOUND('',#1050,.T.);
#576=FACE_OUTER_BOUND('',#1051,.T.);
#577=FACE_OUTER_BOUND('',#1052,.T.);
#578=FACE_OUTER_BOUND('',#1053,.T.);
#579=FACE_OUTER_BOUND('',#1054,.T.);
#580=FACE_OUTER_BOUND('',#1055,.T.);
#581=FACE_OUTER_BOUND('',#1056,.T.);
#582=FACE_OUTER_BOUND('',#1057,.T.);
#583=FACE_OUTER_BOUND('',#1058,.T.);
#584=FACE_OUTER_BOUND('',#1059,.T.);
#585=FACE_OUTER_BOUND('',#1060,.T.);
#586=FACE_OUTER_BOUND('',#1061,.T.);
#587=FACE_OUTER_BOUND('',#1062,.T.);
#588=FACE_OUTER_BOUND('',#1063,.T.);
#589=FACE_OUTER_BOUND('',#1064,.T.);
#590=FACE_OUTER_BOUND('',#1065,.T.);
#591=FACE_OUTER_BOUND('',#1066,.T.);
#592=FACE_OUTER_BOUND('',#1067,.T.);
#593=FACE_OUTER_BOUND('',#1068,.T.);
#594=FACE_OUTER_BOUND('',#1069,.T.);
#595=FACE_OUTER_BOUND('',#1070,.T.);
#596=FACE_OUTER_BOUND('',#1071,.T.);
#597=FACE_OUTER_BOUND('',#1072,.T.);
#598=FACE_OUTER_BOUND('',#1073,.T.);
#599=FACE_OUTER_BOUND('',#1074,.T.);
#600=FACE_OUTER_BOUND('',#1075,.T.);
#601=FACE_OUTER_BOUND('',#1076,.T.);
#602=FACE_OUTER_BOUND('',#1077,.T.);
#603=FACE_OUTER_BOUND('',#1078,.T.);
#604=FACE_OUTER_BOUND('',#1079,.T.);
#605=FACE_OUTER_BOUND('',#1080,.T.);
#606=FACE_OUTER_BOUND('',#1081,.T.);
#607=FACE_OUTER_BOUND('',#1082,.T.);
#608=FACE_OUTER_BOUND('',#1083,.T.);
#609=FACE_OUTER_BOUND('',#1084,.T.);
#610=FACE_OUTER_BOUND('',#1085,.T.);
#611=FACE_OUTER_BOUND('',#1086,.T.);
#612=FACE_OUTER_BOUND('',#1087,.T.);
#613=FACE_OUTER_BOUND('',#1088,.T.);
#614=FACE_OUTER_BOUND('',#1089,.T.);
#615=FACE_OUTER_BOUND('',#1090,.T.);
#616=FACE_OUTER_BOUND('',#1091,.T.);
#617=FACE_OUTER_BOUND('',#1092,.T.);
#618=FACE_OUTER_BOUND('',#1093,.T.);
#619=FACE_OUTER_BOUND('',#1094,.T.);
#620=FACE_OUTER_BOUND('',#1095,.T.);
#621=FACE_OUTER_BOUND('',#1097,.T.);
#622=FACE_OUTER_BOUND('',#1103,.T.);
#623=FACE_OUTER_BOUND('',#1104,.T.);
#624=FACE_OUTER_BOUND('',#1105,.T.);
#625=FACE_OUTER_BOUND('',#1106,.T.);
#626=FACE_OUTER_BOUND('',#1107,.T.);
#627=FACE_OUTER_BOUND('',#1108,.T.);
#628=FACE_OUTER_BOUND('',#1109,.T.);
#629=FACE_OUTER_BOUND('',#1110,.T.);
#630=FACE_OUTER_BOUND('',#1111,.T.);
#631=FACE_OUTER_BOUND('',#1112,.T.);
#632=FACE_OUTER_BOUND('',#1118,.T.);
#633=FACE_OUTER_BOUND('',#1124,.T.);
#634=FACE_OUTER_BOUND('',#1125,.T.);
#635=FACE_OUTER_BOUND('',#1126,.T.);
#636=FACE_OUTER_BOUND('',#1127,.T.);
#637=FACE_OUTER_BOUND('',#1128,.T.);
#638=FACE_OUTER_BOUND('',#1129,.T.);
#639=FACE_OUTER_BOUND('',#1130,.T.);
#640=FACE_OUTER_BOUND('',#1131,.T.);
#641=FACE_OUTER_BOUND('',#1132,.T.);
#642=FACE_OUTER_BOUND('',#1134,.T.);
#643=FACE_OUTER_BOUND('',#1136,.T.);
#644=FACE_OUTER_BOUND('',#1137,.T.);
#645=FACE_OUTER_BOUND('',#1138,.T.);
#646=FACE_OUTER_BOUND('',#1139,.T.);
#647=FACE_OUTER_BOUND('',#1140,.T.);
#648=FACE_OUTER_BOUND('',#1141,.T.);
#649=FACE_OUTER_BOUND('',#1142,.T.);
#650=FACE_OUTER_BOUND('',#1143,.T.);
#651=FACE_OUTER_BOUND('',#1144,.T.);
#652=FACE_OUTER_BOUND('',#1145,.T.);
#653=FACE_OUTER_BOUND('',#1146,.T.);
#654=FACE_OUTER_BOUND('',#1147,.T.);
#655=FACE_OUTER_BOUND('',#1148,.T.);
#656=FACE_OUTER_BOUND('',#1149,.T.);
#657=FACE_OUTER_BOUND('',#1150,.T.);
#658=FACE_OUTER_BOUND('',#1151,.T.);
#659=FACE_OUTER_BOUND('',#1152,.T.);
#660=FACE_OUTER_BOUND('',#1153,.T.);
#661=FACE_OUTER_BOUND('',#1154,.T.);
#662=FACE_OUTER_BOUND('',#1155,.T.);
#663=FACE_OUTER_BOUND('',#1156,.T.);
#664=FACE_OUTER_BOUND('',#1157,.T.);
#665=FACE_OUTER_BOUND('',#1158,.T.);
#666=FACE_OUTER_BOUND('',#1159,.T.);
#667=FACE_OUTER_BOUND('',#1160,.T.);
#668=FACE_OUTER_BOUND('',#1161,.T.);
#669=FACE_OUTER_BOUND('',#1162,.T.);
#670=FACE_OUTER_BOUND('',#1163,.T.);
#671=FACE_OUTER_BOUND('',#1164,.T.);
#672=FACE_OUTER_BOUND('',#1165,.T.);
#673=FACE_OUTER_BOUND('',#1166,.T.);
#674=FACE_OUTER_BOUND('',#1167,.T.);
#675=FACE_OUTER_BOUND('',#1168,.T.);
#676=FACE_OUTER_BOUND('',#1169,.T.);
#677=FACE_OUTER_BOUND('',#1170,.T.);
#678=FACE_OUTER_BOUND('',#1171,.T.);
#679=FACE_OUTER_BOUND('',#1172,.T.);
#680=FACE_OUTER_BOUND('',#1173,.T.);
#681=FACE_OUTER_BOUND('',#1174,.T.);
#682=FACE_OUTER_BOUND('',#1175,.T.);
#683=FACE_OUTER_BOUND('',#1176,.T.);
#684=FACE_OUTER_BOUND('',#1177,.T.);
#685=FACE_OUTER_BOUND('',#1178,.T.);
#686=FACE_OUTER_BOUND('',#1179,.T.);
#687=FACE_OUTER_BOUND('',#1181,.T.);
#688=FACE_OUTER_BOUND('',#1183,.T.);
#689=FACE_OUTER_BOUND('',#1184,.T.);
#690=FACE_OUTER_BOUND('',#1185,.T.);
#691=FACE_OUTER_BOUND('',#1186,.T.);
#692=FACE_OUTER_BOUND('',#1187,.T.);
#693=FACE_OUTER_BOUND('',#1188,.T.);
#694=FACE_OUTER_BOUND('',#1189,.T.);
#695=FACE_OUTER_BOUND('',#1190,.T.);
#696=FACE_OUTER_BOUND('',#1192,.T.);
#697=FACE_OUTER_BOUND('',#1194,.T.);
#698=FACE_OUTER_BOUND('',#1195,.T.);
#699=FACE_OUTER_BOUND('',#1197,.T.);
#700=FACE_OUTER_BOUND('',#1198,.T.);
#701=FACE_OUTER_BOUND('',#1200,.T.);
#702=FACE_OUTER_BOUND('',#1201,.T.);
#703=FACE_OUTER_BOUND('',#1202,.T.);
#704=FACE_OUTER_BOUND('',#1203,.T.);
#705=FACE_OUTER_BOUND('',#1204,.T.);
#706=FACE_OUTER_BOUND('',#1205,.T.);
#707=FACE_OUTER_BOUND('',#1206,.T.);
#708=FACE_OUTER_BOUND('',#1207,.T.);
#709=FACE_OUTER_BOUND('',#1208,.T.);
#710=FACE_OUTER_BOUND('',#1209,.T.);
#711=FACE_OUTER_BOUND('',#1210,.T.);
#712=FACE_OUTER_BOUND('',#1212,.T.);
#713=FACE_OUTER_BOUND('',#1214,.T.);
#714=FACE_OUTER_BOUND('',#1215,.T.);
#715=FACE_OUTER_BOUND('',#1216,.T.);
#716=FACE_OUTER_BOUND('',#1218,.T.);
#717=FACE_OUTER_BOUND('',#1220,.T.);
#718=FACE_OUTER_BOUND('',#1221,.T.);
#719=FACE_OUTER_BOUND('',#1222,.T.);
#720=FACE_OUTER_BOUND('',#1223,.T.);
#721=FACE_OUTER_BOUND('',#1224,.T.);
#722=FACE_OUTER_BOUND('',#1225,.T.);
#723=FACE_OUTER_BOUND('',#1226,.T.);
#724=FACE_OUTER_BOUND('',#1227,.T.);
#725=FACE_OUTER_BOUND('',#1228,.T.);
#726=FACE_OUTER_BOUND('',#1230,.T.);
#727=FACE_OUTER_BOUND('',#1232,.T.);
#728=FACE_OUTER_BOUND('',#1233,.T.);
#729=FACE_OUTER_BOUND('',#1234,.T.);
#730=FACE_OUTER_BOUND('',#1235,.T.);
#731=FACE_OUTER_BOUND('',#1236,.T.);
#732=FACE_OUTER_BOUND('',#1237,.T.);
#733=FACE_OUTER_BOUND('',#1238,.T.);
#734=FACE_OUTER_BOUND('',#1239,.T.);
#735=FACE_OUTER_BOUND('',#1240,.T.);
#736=FACE_OUTER_BOUND('',#1241,.T.);
#737=FACE_OUTER_BOUND('',#1242,.T.);
#738=FACE_OUTER_BOUND('',#1243,.T.);
#739=FACE_OUTER_BOUND('',#1244,.T.);
#740=FACE_OUTER_BOUND('',#1245,.T.);
#741=FACE_OUTER_BOUND('',#1246,.T.);
#742=FACE_OUTER_BOUND('',#1247,.T.);
#743=FACE_OUTER_BOUND('',#1248,.T.);
#744=FACE_OUTER_BOUND('',#1249,.T.);
#745=FACE_OUTER_BOUND('',#1250,.T.);
#746=FACE_OUTER_BOUND('',#1251,.T.);
#747=FACE_OUTER_BOUND('',#1252,.T.);
#748=FACE_OUTER_BOUND('',#1253,.T.);
#749=FACE_OUTER_BOUND('',#1254,.T.);
#750=FACE_OUTER_BOUND('',#1255,.T.);
#751=FACE_OUTER_BOUND('',#1256,.T.);
#752=FACE_OUTER_BOUND('',#1257,.T.);
#753=FACE_OUTER_BOUND('',#1258,.T.);
#754=FACE_OUTER_BOUND('',#1259,.T.);
#755=FACE_OUTER_BOUND('',#1260,.T.);
#756=FACE_OUTER_BOUND('',#1261,.T.);
#757=FACE_OUTER_BOUND('',#1262,.T.);
#758=FACE_OUTER_BOUND('',#1263,.T.);
#759=FACE_OUTER_BOUND('',#1264,.T.);
#760=FACE_OUTER_BOUND('',#1266,.T.);
#761=FACE_OUTER_BOUND('',#1267,.T.);
#762=FACE_OUTER_BOUND('',#1269,.T.);
#763=FACE_OUTER_BOUND('',#1270,.T.);
#764=FACE_OUTER_BOUND('',#1271,.T.);
#765=FACE_OUTER_BOUND('',#1274,.T.);
#766=FACE_OUTER_BOUND('',#1275,.T.);
#767=FACE_OUTER_BOUND('',#1276,.T.);
#768=FACE_OUTER_BOUND('',#1277,.T.);
#769=FACE_OUTER_BOUND('',#1278,.T.);
#770=FACE_OUTER_BOUND('',#1280,.T.);
#771=FACE_OUTER_BOUND('',#1282,.T.);
#772=FACE_OUTER_BOUND('',#1283,.T.);
#773=FACE_OUTER_BOUND('',#1284,.T.);
#774=FACE_OUTER_BOUND('',#1286,.T.);
#775=FACE_OUTER_BOUND('',#1288,.T.);
#776=FACE_OUTER_BOUND('',#1289,.T.);
#777=FACE_OUTER_BOUND('',#1292,.T.);
#778=FACE_OUTER_BOUND('',#1293,.T.);
#779=FACE_OUTER_BOUND('',#1295,.T.);
#780=FACE_OUTER_BOUND('',#1297,.T.);
#781=FACE_OUTER_BOUND('',#1298,.T.);
#782=FACE_OUTER_BOUND('',#1300,.T.);
#783=FACE_OUTER_BOUND('',#1301,.T.);
#784=FACE_OUTER_BOUND('',#1302,.T.);
#785=FACE_OUTER_BOUND('',#1303,.T.);
#786=FACE_OUTER_BOUND('',#1304,.T.);
#787=FACE_OUTER_BOUND('',#1305,.T.);
#788=FACE_OUTER_BOUND('',#1306,.T.);
#789=FACE_OUTER_BOUND('',#1307,.T.);
#790=FACE_OUTER_BOUND('',#1308,.T.);
#791=FACE_OUTER_BOUND('',#1309,.T.);
#792=FACE_OUTER_BOUND('',#1310,.T.);
#793=FACE_OUTER_BOUND('',#1311,.T.);
#794=FACE_OUTER_BOUND('',#1312,.T.);
#795=FACE_OUTER_BOUND('',#1315,.T.);
#796=FACE_OUTER_BOUND('',#1316,.T.);
#797=FACE_OUTER_BOUND('',#1317,.T.);
#798=FACE_OUTER_BOUND('',#1318,.T.);
#799=FACE_OUTER_BOUND('',#1320,.T.);
#800=FACE_OUTER_BOUND('',#1321,.T.);
#801=FACE_OUTER_BOUND('',#1322,.T.);
#802=FACE_OUTER_BOUND('',#1324,.T.);
#803=FACE_OUTER_BOUND('',#1325,.T.);
#804=FACE_OUTER_BOUND('',#1326,.T.);
#805=FACE_OUTER_BOUND('',#1329,.T.);
#806=FACE_OUTER_BOUND('',#1330,.T.);
#807=FACE_OUTER_BOUND('',#1331,.T.);
#808=FACE_OUTER_BOUND('',#1333,.T.);
#809=FACE_OUTER_BOUND('',#1335,.T.);
#810=FACE_OUTER_BOUND('',#1336,.T.);
#811=FACE_OUTER_BOUND('',#1337,.T.);
#812=FACE_OUTER_BOUND('',#1338,.T.);
#813=FACE_OUTER_BOUND('',#1339,.T.);
#814=FACE_OUTER_BOUND('',#1340,.T.);
#815=FACE_OUTER_BOUND('',#1341,.T.);
#816=FACE_OUTER_BOUND('',#1342,.T.);
#817=FACE_OUTER_BOUND('',#1343,.T.);
#818=FACE_OUTER_BOUND('',#1344,.T.);
#819=FACE_OUTER_BOUND('',#1345,.T.);
#820=FACE_OUTER_BOUND('',#1346,.T.);
#821=FACE_OUTER_BOUND('',#1347,.T.);
#822=FACE_OUTER_BOUND('',#1348,.T.);
#823=FACE_OUTER_BOUND('',#1349,.T.);
#824=FACE_OUTER_BOUND('',#1350,.T.);
#825=FACE_OUTER_BOUND('',#1351,.T.);
#826=FACE_OUTER_BOUND('',#1352,.T.);
#827=FACE_OUTER_BOUND('',#1353,.T.);
#828=FACE_OUTER_BOUND('',#1354,.T.);
#829=FACE_OUTER_BOUND('',#1355,.T.);
#830=FACE_OUTER_BOUND('',#1356,.T.);
#831=FACE_OUTER_BOUND('',#1357,.T.);
#832=FACE_OUTER_BOUND('',#1358,.T.);
#833=FACE_OUTER_BOUND('',#1359,.T.);
#834=FACE_OUTER_BOUND('',#1360,.T.);
#835=FACE_OUTER_BOUND('',#1361,.T.);
#836=FACE_OUTER_BOUND('',#1362,.T.);
#837=FACE_OUTER_BOUND('',#1363,.T.);
#838=FACE_OUTER_BOUND('',#1364,.T.);
#839=FACE_OUTER_BOUND('',#1365,.T.);
#840=FACE_OUTER_BOUND('',#1366,.T.);
#841=FACE_OUTER_BOUND('',#1367,.T.);
#842=FACE_OUTER_BOUND('',#1368,.T.);
#843=FACE_OUTER_BOUND('',#1369,.T.);
#844=FACE_OUTER_BOUND('',#1370,.T.);
#845=FACE_OUTER_BOUND('',#1371,.T.);
#846=FACE_OUTER_BOUND('',#1372,.T.);
#847=FACE_OUTER_BOUND('',#1373,.T.);
#848=FACE_OUTER_BOUND('',#1374,.T.);
#849=FACE_OUTER_BOUND('',#1375,.T.);
#850=FACE_OUTER_BOUND('',#1376,.T.);
#851=FACE_OUTER_BOUND('',#1377,.T.);
#852=FACE_OUTER_BOUND('',#1378,.T.);
#853=FACE_OUTER_BOUND('',#1379,.T.);
#854=FACE_OUTER_BOUND('',#1380,.T.);
#855=FACE_OUTER_BOUND('',#1381,.T.);
#856=FACE_OUTER_BOUND('',#1382,.T.);
#857=FACE_OUTER_BOUND('',#1383,.T.);
#858=FACE_OUTER_BOUND('',#1384,.T.);
#859=FACE_OUTER_BOUND('',#1385,.T.);
#860=FACE_OUTER_BOUND('',#1387,.T.);
#861=FACE_OUTER_BOUND('',#1388,.T.);
#862=FACE_OUTER_BOUND('',#1390,.T.);
#863=FACE_OUTER_BOUND('',#1391,.T.);
#864=FACE_OUTER_BOUND('',#1392,.T.);
#865=FACE_OUTER_BOUND('',#1393,.T.);
#866=FACE_OUTER_BOUND('',#1394,.T.);
#867=FACE_OUTER_BOUND('',#1395,.T.);
#868=FACE_OUTER_BOUND('',#1396,.T.);
#869=FACE_OUTER_BOUND('',#1397,.T.);
#870=FACE_OUTER_BOUND('',#1398,.T.);
#871=FACE_OUTER_BOUND('',#1399,.T.);
#872=FACE_OUTER_BOUND('',#1400,.T.);
#873=FACE_OUTER_BOUND('',#1401,.T.);
#874=FACE_OUTER_BOUND('',#1402,.T.);
#875=FACE_OUTER_BOUND('',#1403,.T.);
#876=FACE_OUTER_BOUND('',#1404,.T.);
#877=FACE_OUTER_BOUND('',#1405,.T.);
#878=FACE_OUTER_BOUND('',#1406,.T.);
#879=FACE_OUTER_BOUND('',#1407,.T.);
#880=FACE_OUTER_BOUND('',#1408,.T.);
#881=FACE_OUTER_BOUND('',#1409,.T.);
#882=FACE_OUTER_BOUND('',#1410,.T.);
#883=FACE_OUTER_BOUND('',#1411,.T.);
#884=FACE_OUTER_BOUND('',#1412,.T.);
#885=FACE_OUTER_BOUND('',#1413,.T.);
#886=FACE_OUTER_BOUND('',#1414,.T.);
#887=FACE_OUTER_BOUND('',#1415,.T.);
#888=FACE_OUTER_BOUND('',#1416,.T.);
#889=FACE_OUTER_BOUND('',#1417,.T.);
#890=FACE_OUTER_BOUND('',#1418,.T.);
#891=FACE_OUTER_BOUND('',#1419,.T.);
#892=FACE_OUTER_BOUND('',#1420,.T.);
#893=FACE_OUTER_BOUND('',#1421,.T.);
#894=FACE_OUTER_BOUND('',#1422,.T.);
#895=FACE_OUTER_BOUND('',#1423,.T.);
#896=FACE_OUTER_BOUND('',#1424,.T.);
#897=FACE_OUTER_BOUND('',#1425,.T.);
#898=FACE_OUTER_BOUND('',#1427,.T.);
#899=FACE_OUTER_BOUND('',#1428,.T.);
#900=FACE_OUTER_BOUND('',#1430,.T.);
#901=FACE_OUTER_BOUND('',#1431,.T.);
#902=FACE_OUTER_BOUND('',#1432,.T.);
#903=FACE_OUTER_BOUND('',#1433,.T.);
#904=FACE_OUTER_BOUND('',#1435,.T.);
#905=FACE_OUTER_BOUND('',#1437,.T.);
#906=FACE_OUTER_BOUND('',#1438,.T.);
#907=FACE_OUTER_BOUND('',#1439,.T.);
#908=FACE_OUTER_BOUND('',#1440,.T.);
#909=FACE_OUTER_BOUND('',#1441,.T.);
#910=FACE_OUTER_BOUND('',#1442,.T.);
#911=FACE_OUTER_BOUND('',#1443,.T.);
#912=FACE_OUTER_BOUND('',#1444,.T.);
#913=FACE_OUTER_BOUND('',#1445,.T.);
#914=FACE_OUTER_BOUND('',#1446,.T.);
#915=FACE_OUTER_BOUND('',#1447,.T.);
#916=FACE_OUTER_BOUND('',#1448,.T.);
#917=FACE_OUTER_BOUND('',#1449,.T.);
#918=FACE_OUTER_BOUND('',#1450,.T.);
#919=FACE_OUTER_BOUND('',#1452,.T.);
#920=FACE_OUTER_BOUND('',#1453,.T.);
#921=FACE_OUTER_BOUND('',#1454,.T.);
#922=FACE_OUTER_BOUND('',#1455,.T.);
#923=FACE_OUTER_BOUND('',#1456,.T.);
#924=FACE_OUTER_BOUND('',#1457,.T.);
#925=FACE_OUTER_BOUND('',#1458,.T.);
#926=FACE_OUTER_BOUND('',#1459,.T.);
#927=EDGE_LOOP('',(#5367,#5368,#5369,#5370,#5371,#5372,#5373,#5374));
#928=EDGE_LOOP('',(#5375,#5376,#5377,#5378));
#929=EDGE_LOOP('',(#5379,#5380,#5381,#5382));
#930=EDGE_LOOP('',(#5383,#5384,#5385,#5386));
#931=EDGE_LOOP('',(#5387,#5388,#5389,#5390));
#932=EDGE_LOOP('',(#5391,#5392,#5393,#5394));
#933=EDGE_LOOP('',(#5395,#5396,#5397,#5398));
#934=EDGE_LOOP('',(#5399,#5400,#5401,#5402));
#935=EDGE_LOOP('',(#5403,#5404,#5405,#5406));
#936=EDGE_LOOP('',(#5407,#5408,#5409,#5410));
#937=EDGE_LOOP('',(#5411,#5412,#5413,#5414));
#938=EDGE_LOOP('',(#5415,#5416,#5417,#5418));
#939=EDGE_LOOP('',(#5419,#5420,#5421,#5422));
#940=EDGE_LOOP('',(#5423,#5424,#5425,#5426));
#941=EDGE_LOOP('',(#5427,#5428,#5429,#5430));
#942=EDGE_LOOP('',(#5431,#5432,#5433,#5434));
#943=EDGE_LOOP('',(#5435,#5436,#5437,#5438));
#944=EDGE_LOOP('',(#5439,#5440,#5441,#5442));
#945=EDGE_LOOP('',(#5443,#5444,#5445,#5446));
#946=EDGE_LOOP('',(#5447,#5448,#5449,#5450));
#947=EDGE_LOOP('',(#5451,#5452,#5453,#5454));
#948=EDGE_LOOP('',(#5455,#5456,#5457,#5458));
#949=EDGE_LOOP('',(#5459,#5460,#5461,#5462));
#950=EDGE_LOOP('',(#5463,#5464,#5465,#5466));
#951=EDGE_LOOP('',(#5467,#5468,#5469,#5470));
#952=EDGE_LOOP('',(#5471,#5472,#5473,#5474));
#953=EDGE_LOOP('',(#5475,#5476,#5477,#5478));
#954=EDGE_LOOP('',(#5479,#5480,#5481,#5482));
#955=EDGE_LOOP('',(#5483,#5484,#5485,#5486));
#956=EDGE_LOOP('',(#5487,#5488,#5489,#5490));
#957=EDGE_LOOP('',(#5491,#5492,#5493,#5494));
#958=EDGE_LOOP('',(#5495,#5496,#5497,#5498));
#959=EDGE_LOOP('',(#5499,#5500,#5501,#5502));
#960=EDGE_LOOP('',(#5503,#5504,#5505,#5506));
#961=EDGE_LOOP('',(#5507,#5508,#5509,#5510,#5511,#5512,#5513,#5514));
#962=EDGE_LOOP('',(#5515,#5516,#5517,#5518));
#963=EDGE_LOOP('',(#5519,#5520,#5521,#5522));
#964=EDGE_LOOP('',(#5523,#5524,#5525,#5526));
#965=EDGE_LOOP('',(#5527,#5528,#5529,#5530));
#966=EDGE_LOOP('',(#5531,#5532,#5533,#5534));
#967=EDGE_LOOP('',(#5535,#5536,#5537,#5538));
#968=EDGE_LOOP('',(#5539,#5540,#5541,#5542));
#969=EDGE_LOOP('',(#5543,#5544,#5545,#5546));
#970=EDGE_LOOP('',(#5547,#5548,#5549,#5550));
#971=EDGE_LOOP('',(#5551,#5552,#5553,#5554));
#972=EDGE_LOOP('',(#5555,#5556,#5557,#5558));
#973=EDGE_LOOP('',(#5559,#5560,#5561,#5562));
#974=EDGE_LOOP('',(#5563,#5564,#5565,#5566));
#975=EDGE_LOOP('',(#5567,#5568,#5569,#5570));
#976=EDGE_LOOP('',(#5571,#5572,#5573,#5574));
#977=EDGE_LOOP('',(#5575,#5576,#5577,#5578));
#978=EDGE_LOOP('',(#5579,#5580,#5581,#5582));
#979=EDGE_LOOP('',(#5583,#5584,#5585,#5586));
#980=EDGE_LOOP('',(#5587,#5588,#5589,#5590));
#981=EDGE_LOOP('',(#5591,#5592,#5593,#5594));
#982=EDGE_LOOP('',(#5595,#5596,#5597,#5598));
#983=EDGE_LOOP('',(#5599,#5600,#5601,#5602));
#984=EDGE_LOOP('',(#5603,#5604,#5605,#5606));
#985=EDGE_LOOP('',(#5607,#5608,#5609,#5610));
#986=EDGE_LOOP('',(#5611,#5612,#5613,#5614));
#987=EDGE_LOOP('',(#5615,#5616,#5617,#5618));
#988=EDGE_LOOP('',(#5619,#5620,#5621,#5622));
#989=EDGE_LOOP('',(#5623,#5624,#5625,#5626));
#990=EDGE_LOOP('',(#5627,#5628,#5629,#5630));
#991=EDGE_LOOP('',(#5631,#5632,#5633,#5634));
#992=EDGE_LOOP('',(#5635,#5636,#5637,#5638));
#993=EDGE_LOOP('',(#5639,#5640,#5641,#5642));
#994=EDGE_LOOP('',(#5643,#5644,#5645,#5646));
#995=EDGE_LOOP('',(#5647,#5648,#5649,#5650,#5651,#5652,#5653,#5654));
#996=EDGE_LOOP('',(#5655,#5656,#5657,#5658));
#997=EDGE_LOOP('',(#5659,#5660,#5661,#5662));
#998=EDGE_LOOP('',(#5663,#5664,#5665,#5666));
#999=EDGE_LOOP('',(#5667,#5668,#5669,#5670));
#1000=EDGE_LOOP('',(#5671,#5672,#5673,#5674));
#1001=EDGE_LOOP('',(#5675,#5676,#5677,#5678));
#1002=EDGE_LOOP('',(#5679,#5680,#5681,#5682));
#1003=EDGE_LOOP('',(#5683,#5684,#5685,#5686));
#1004=EDGE_LOOP('',(#5687,#5688,#5689,#5690));
#1005=EDGE_LOOP('',(#5691,#5692,#5693,#5694));
#1006=EDGE_LOOP('',(#5695,#5696,#5697,#5698));
#1007=EDGE_LOOP('',(#5699,#5700,#5701,#5702));
#1008=EDGE_LOOP('',(#5703,#5704,#5705,#5706));
#1009=EDGE_LOOP('',(#5707,#5708,#5709,#5710));
#1010=EDGE_LOOP('',(#5711,#5712,#5713,#5714));
#1011=EDGE_LOOP('',(#5715,#5716,#5717,#5718));
#1012=EDGE_LOOP('',(#5719,#5720,#5721,#5722));
#1013=EDGE_LOOP('',(#5723,#5724,#5725,#5726));
#1014=EDGE_LOOP('',(#5727,#5728,#5729,#5730));
#1015=EDGE_LOOP('',(#5731,#5732,#5733,#5734));
#1016=EDGE_LOOP('',(#5735,#5736,#5737,#5738));
#1017=EDGE_LOOP('',(#5739,#5740,#5741,#5742));
#1018=EDGE_LOOP('',(#5743,#5744,#5745,#5746));
#1019=EDGE_LOOP('',(#5747,#5748,#5749,#5750));
#1020=EDGE_LOOP('',(#5751,#5752,#5753,#5754));
#1021=EDGE_LOOP('',(#5755,#5756,#5757,#5758));
#1022=EDGE_LOOP('',(#5759,#5760,#5761,#5762));
#1023=EDGE_LOOP('',(#5763,#5764,#5765,#5766));
#1024=EDGE_LOOP('',(#5767,#5768,#5769,#5770));
#1025=EDGE_LOOP('',(#5771,#5772,#5773,#5774));
#1026=EDGE_LOOP('',(#5775,#5776,#5777,#5778));
#1027=EDGE_LOOP('',(#5779,#5780,#5781,#5782));
#1028=EDGE_LOOP('',(#5783,#5784,#5785,#5786));
#1029=EDGE_LOOP('',(#5787,#5788,#5789,#5790,#5791,#5792,#5793,#5794));
#1030=EDGE_LOOP('',(#5795,#5796,#5797,#5798));
#1031=EDGE_LOOP('',(#5799,#5800,#5801,#5802));
#1032=EDGE_LOOP('',(#5803,#5804,#5805,#5806));
#1033=EDGE_LOOP('',(#5807,#5808,#5809,#5810));
#1034=EDGE_LOOP('',(#5811,#5812,#5813,#5814));
#1035=EDGE_LOOP('',(#5815,#5816,#5817,#5818));
#1036=EDGE_LOOP('',(#5819,#5820,#5821,#5822));
#1037=EDGE_LOOP('',(#5823,#5824,#5825,#5826));
#1038=EDGE_LOOP('',(#5827,#5828,#5829,#5830));
#1039=EDGE_LOOP('',(#5831,#5832,#5833,#5834));
#1040=EDGE_LOOP('',(#5835,#5836,#5837,#5838));
#1041=EDGE_LOOP('',(#5839,#5840,#5841,#5842));
#1042=EDGE_LOOP('',(#5843,#5844,#5845,#5846));
#1043=EDGE_LOOP('',(#5847,#5848,#5849,#5850));
#1044=EDGE_LOOP('',(#5851,#5852,#5853,#5854));
#1045=EDGE_LOOP('',(#5855,#5856,#5857,#5858));
#1046=EDGE_LOOP('',(#5859,#5860,#5861,#5862));
#1047=EDGE_LOOP('',(#5863,#5864,#5865,#5866));
#1048=EDGE_LOOP('',(#5867,#5868,#5869,#5870));
#1049=EDGE_LOOP('',(#5871,#5872,#5873,#5874));
#1050=EDGE_LOOP('',(#5875,#5876,#5877,#5878));
#1051=EDGE_LOOP('',(#5879,#5880,#5881,#5882));
#1052=EDGE_LOOP('',(#5883,#5884,#5885,#5886));
#1053=EDGE_LOOP('',(#5887,#5888,#5889,#5890));
#1054=EDGE_LOOP('',(#5891,#5892,#5893,#5894));
#1055=EDGE_LOOP('',(#5895,#5896,#5897,#5898));
#1056=EDGE_LOOP('',(#5899,#5900,#5901,#5902));
#1057=EDGE_LOOP('',(#5903,#5904,#5905,#5906));
#1058=EDGE_LOOP('',(#5907,#5908,#5909,#5910));
#1059=EDGE_LOOP('',(#5911,#5912,#5913,#5914));
#1060=EDGE_LOOP('',(#5915,#5916,#5917,#5918));
#1061=EDGE_LOOP('',(#5919,#5920,#5921,#5922));
#1062=EDGE_LOOP('',(#5923,#5924,#5925,#5926));
#1063=EDGE_LOOP('',(#5927,#5928,#5929,#5930,#5931));
#1064=EDGE_LOOP('',(#5932,#5933,#5934,#5935));
#1065=EDGE_LOOP('',(#5936,#5937,#5938,#5939,#5940,#5941,#5942,#5943,#5944,
#5945,#5946,#5947,#5948,#5949,#5950,#5951,#5952,#5953,#5954,#5955,#5956,
#5957,#5958,#5959,#5960,#5961,#5962,#5963,#5964,#5965,#5966,#5967,#5968,
#5969,#5970,#5971,#5972,#5973));
#1066=EDGE_LOOP('',(#5974,#5975,#5976,#5977,#5978,#5979,#5980,#5981,#5982,
#5983,#5984,#5985,#5986,#5987,#5988,#5989,#5990,#5991,#5992,#5993,#5994,
#5995,#5996,#5997,#5998,#5999,#6000,#6001,#6002,#6003,#6004,#6005,#6006,
#6007,#6008,#6009,#6010,#6011));
#1067=EDGE_LOOP('',(#6012,#6013,#6014,#6015));
#1068=EDGE_LOOP('',(#6016,#6017,#6018,#6019,#6020));
#1069=EDGE_LOOP('',(#6021,#6022,#6023,#6024));
#1070=EDGE_LOOP('',(#6025,#6026,#6027,#6028,#6029,#6030,#6031,#6032,#6033,
#6034,#6035,#6036,#6037,#6038,#6039,#6040,#6041,#6042,#6043,#6044,#6045,
#6046,#6047,#6048,#6049,#6050,#6051,#6052,#6053,#6054,#6055,#6056,#6057,
#6058,#6059,#6060,#6061,#6062));
#1071=EDGE_LOOP('',(#6063,#6064,#6065,#6066,#6067,#6068,#6069,#6070,#6071,
#6072,#6073,#6074,#6075,#6076,#6077,#6078,#6079,#6080,#6081,#6082,#6083,
#6084,#6085,#6086,#6087,#6088,#6089,#6090,#6091,#6092,#6093,#6094,#6095,
#6096,#6097,#6098,#6099,#6100));
#1072=EDGE_LOOP('',(#6101,#6102,#6103,#6104));
#1073=EDGE_LOOP('',(#6105,#6106,#6107,#6108,#6109));
#1074=EDGE_LOOP('',(#6110,#6111,#6112,#6113));
#1075=EDGE_LOOP('',(#6114,#6115,#6116,#6117,#6118,#6119,#6120,#6121,#6122,
#6123,#6124,#6125,#6126,#6127,#6128,#6129,#6130,#6131,#6132,#6133,#6134,
#6135,#6136,#6137,#6138,#6139,#6140,#6141,#6142,#6143,#6144,#6145,#6146,
#6147,#6148,#6149,#6150,#6151));
#1076=EDGE_LOOP('',(#6152,#6153,#6154,#6155,#6156,#6157,#6158,#6159,#6160,
#6161,#6162,#6163,#6164,#6165,#6166,#6167,#6168,#6169,#6170,#6171,#6172,
#6173,#6174,#6175,#6176,#6177,#6178,#6179,#6180,#6181,#6182,#6183,#6184,
#6185,#6186,#6187,#6188,#6189));
#1077=EDGE_LOOP('',(#6190,#6191,#6192,#6193));
#1078=EDGE_LOOP('',(#6194,#6195,#6196,#6197,#6198));
#1079=EDGE_LOOP('',(#6199,#6200,#6201,#6202));
#1080=EDGE_LOOP('',(#6203,#6204,#6205,#6206,#6207,#6208,#6209,#6210,#6211,
#6212,#6213,#6214,#6215,#6216,#6217,#6218,#6219,#6220,#6221,#6222,#6223,
#6224,#6225,#6226,#6227,#6228,#6229,#6230,#6231,#6232,#6233,#6234,#6235,
#6236,#6237,#6238,#6239,#6240));
#1081=EDGE_LOOP('',(#6241,#6242,#6243,#6244,#6245,#6246,#6247,#6248,#6249,
#6250,#6251,#6252,#6253,#6254,#6255,#6256,#6257,#6258,#6259,#6260,#6261,
#6262,#6263,#6264,#6265,#6266,#6267,#6268,#6269,#6270,#6271,#6272,#6273,
#6274,#6275,#6276,#6277,#6278));
#1082=EDGE_LOOP('',(#6279,#6280,#6281,#6282));
#1083=EDGE_LOOP('',(#6283));
#1084=EDGE_LOOP('',(#6284));
#1085=EDGE_LOOP('',(#6285));
#1086=EDGE_LOOP('',(#6286));
#1087=EDGE_LOOP('',(#6287,#6288,#6289,#6290));
#1088=EDGE_LOOP('',(#6291,#6292,#6293,#6294));
#1089=EDGE_LOOP('',(#6295,#6296,#6297,#6298));
#1090=EDGE_LOOP('',(#6299,#6300,#6301,#6302));
#1091=EDGE_LOOP('',(#6303,#6304,#6305,#6306));
#1092=EDGE_LOOP('',(#6307,#6308,#6309,#6310));
#1093=EDGE_LOOP('',(#6311,#6312,#6313,#6314));
#1094=EDGE_LOOP('',(#6315,#6316,#6317,#6318));
#1095=EDGE_LOOP('',(#6319,#6320,#6321,#6322));
#1096=EDGE_LOOP('',(#6323,#6324,#6325,#6326));
#1097=EDGE_LOOP('',(#6327,#6328,#6329,#6330));
#1098=EDGE_LOOP('',(#6331,#6332,#6333,#6334));
#1099=EDGE_LOOP('',(#6335,#6336,#6337,#6338));
#1100=EDGE_LOOP('',(#6339,#6340,#6341,#6342));
#1101=EDGE_LOOP('',(#6343,#6344,#6345,#6346));
#1102=EDGE_LOOP('',(#6347,#6348,#6349,#6350));
#1103=EDGE_LOOP('',(#6351,#6352,#6353,#6354));
#1104=EDGE_LOOP('',(#6355,#6356,#6357,#6358));
#1105=EDGE_LOOP('',(#6359,#6360,#6361,#6362));
#1106=EDGE_LOOP('',(#6363,#6364,#6365,#6366));
#1107=EDGE_LOOP('',(#6367,#6368,#6369,#6370));
#1108=EDGE_LOOP('',(#6371,#6372,#6373,#6374));
#1109=EDGE_LOOP('',(#6375,#6376,#6377,#6378));
#1110=EDGE_LOOP('',(#6379,#6380,#6381,#6382));
#1111=EDGE_LOOP('',(#6383,#6384,#6385,#6386));
#1112=EDGE_LOOP('',(#6387,#6388,#6389,#6390));
#1113=EDGE_LOOP('',(#6391));
#1114=EDGE_LOOP('',(#6392));
#1115=EDGE_LOOP('',(#6393));
#1116=EDGE_LOOP('',(#6394));
#1117=EDGE_LOOP('',(#6395));
#1118=EDGE_LOOP('',(#6396,#6397,#6398,#6399));
#1119=EDGE_LOOP('',(#6400));
#1120=EDGE_LOOP('',(#6401));
#1121=EDGE_LOOP('',(#6402));
#1122=EDGE_LOOP('',(#6403));
#1123=EDGE_LOOP('',(#6404));
#1124=EDGE_LOOP('',(#6405,#6406,#6407,#6408));
#1125=EDGE_LOOP('',(#6409,#6410,#6411,#6412));
#1126=EDGE_LOOP('',(#6413,#6414,#6415,#6416));
#1127=EDGE_LOOP('',(#6417,#6418,#6419,#6420));
#1128=EDGE_LOOP('',(#6421,#6422,#6423,#6424));
#1129=EDGE_LOOP('',(#6425,#6426,#6427,#6428));
#1130=EDGE_LOOP('',(#6429,#6430,#6431,#6432));
#1131=EDGE_LOOP('',(#6433,#6434,#6435,#6436));
#1132=EDGE_LOOP('',(#6437,#6438,#6439,#6440));
#1133=EDGE_LOOP('',(#6441,#6442,#6443,#6444));
#1134=EDGE_LOOP('',(#6445,#6446,#6447,#6448));
#1135=EDGE_LOOP('',(#6449,#6450,#6451,#6452));
#1136=EDGE_LOOP('',(#6453,#6454,#6455,#6456,#6457,#6458,#6459,#6460));
#1137=EDGE_LOOP('',(#6461,#6462,#6463,#6464));
#1138=EDGE_LOOP('',(#6465,#6466,#6467,#6468));
#1139=EDGE_LOOP('',(#6469,#6470,#6471,#6472));
#1140=EDGE_LOOP('',(#6473,#6474,#6475,#6476));
#1141=EDGE_LOOP('',(#6477,#6478,#6479,#6480));
#1142=EDGE_LOOP('',(#6481,#6482,#6483,#6484));
#1143=EDGE_LOOP('',(#6485,#6486,#6487,#6488));
#1144=EDGE_LOOP('',(#6489,#6490,#6491,#6492));
#1145=EDGE_LOOP('',(#6493,#6494,#6495,#6496));
#1146=EDGE_LOOP('',(#6497,#6498,#6499,#6500));
#1147=EDGE_LOOP('',(#6501,#6502,#6503,#6504));
#1148=EDGE_LOOP('',(#6505,#6506,#6507,#6508));
#1149=EDGE_LOOP('',(#6509,#6510,#6511,#6512));
#1150=EDGE_LOOP('',(#6513,#6514,#6515,#6516));
#1151=EDGE_LOOP('',(#6517,#6518,#6519,#6520));
#1152=EDGE_LOOP('',(#6521,#6522,#6523,#6524));
#1153=EDGE_LOOP('',(#6525,#6526,#6527,#6528));
#1154=EDGE_LOOP('',(#6529,#6530,#6531,#6532));
#1155=EDGE_LOOP('',(#6533,#6534,#6535,#6536));
#1156=EDGE_LOOP('',(#6537,#6538,#6539,#6540));
#1157=EDGE_LOOP('',(#6541,#6542,#6543,#6544));
#1158=EDGE_LOOP('',(#6545,#6546,#6547,#6548));
#1159=EDGE_LOOP('',(#6549,#6550,#6551,#6552));
#1160=EDGE_LOOP('',(#6553,#6554,#6555,#6556));
#1161=EDGE_LOOP('',(#6557,#6558,#6559,#6560));
#1162=EDGE_LOOP('',(#6561,#6562,#6563,#6564));
#1163=EDGE_LOOP('',(#6565,#6566,#6567,#6568));
#1164=EDGE_LOOP('',(#6569,#6570,#6571,#6572));
#1165=EDGE_LOOP('',(#6573,#6574,#6575,#6576));
#1166=EDGE_LOOP('',(#6577,#6578,#6579,#6580));
#1167=EDGE_LOOP('',(#6581,#6582,#6583,#6584));
#1168=EDGE_LOOP('',(#6585,#6586,#6587,#6588));
#1169=EDGE_LOOP('',(#6589,#6590,#6591,#6592,#6593,#6594,#6595,#6596,#6597,
#6598,#6599,#6600,#6601,#6602,#6603,#6604,#6605,#6606,#6607,#6608,#6609,
#6610,#6611,#6612,#6613,#6614,#6615,#6616,#6617,#6618,#6619,#6620,#6621,
#6622,#6623,#6624));
#1170=EDGE_LOOP('',(#6625,#6626,#6627,#6628,#6629,#6630,#6631,#6632,#6633,
#6634,#6635,#6636,#6637,#6638,#6639,#6640,#6641,#6642,#6643,#6644,#6645,
#6646,#6647,#6648,#6649,#6650,#6651,#6652,#6653,#6654,#6655,#6656,#6657,
#6658,#6659));
#1171=EDGE_LOOP('',(#6660,#6661,#6662,#6663));
#1172=EDGE_LOOP('',(#6664));
#1173=EDGE_LOOP('',(#6665,#6666,#6667,#6668));
#1174=EDGE_LOOP('',(#6669,#6670,#6671,#6672));
#1175=EDGE_LOOP('',(#6673,#6674,#6675,#6676));
#1176=EDGE_LOOP('',(#6677,#6678,#6679,#6680));
#1177=EDGE_LOOP('',(#6681,#6682,#6683,#6684));
#1178=EDGE_LOOP('',(#6685,#6686,#6687,#6688));
#1179=EDGE_LOOP('',(#6689));
#1180=EDGE_LOOP('',(#6690));
#1181=EDGE_LOOP('',(#6691));
#1182=EDGE_LOOP('',(#6692));
#1183=EDGE_LOOP('',(#6693,#6694,#6695,#6696));
#1184=EDGE_LOOP('',(#6697,#6698,#6699,#6700));
#1185=EDGE_LOOP('',(#6701,#6702,#6703,#6704));
#1186=EDGE_LOOP('',(#6705,#6706,#6707,#6708));
#1187=EDGE_LOOP('',(#6709,#6710,#6711,#6712));
#1188=EDGE_LOOP('',(#6713,#6714,#6715,#6716));
#1189=EDGE_LOOP('',(#6717,#6718,#6719,#6720));
#1190=EDGE_LOOP('',(#6721,#6722,#6723,#6724,#6725,#6726));
#1191=EDGE_LOOP('',(#6727,#6728,#6729,#6730));
#1192=EDGE_LOOP('',(#6731));
#1193=EDGE_LOOP('',(#6732));
#1194=EDGE_LOOP('',(#6733,#6734,#6735,#6736));
#1195=EDGE_LOOP('',(#6737));
#1196=EDGE_LOOP('',(#6738,#6739,#6740,#6741));
#1197=EDGE_LOOP('',(#6742,#6743,#6744,#6745));
#1198=EDGE_LOOP('',(#6746));
#1199=EDGE_LOOP('',(#6747,#6748,#6749,#6750,#6751,#6752));
#1200=EDGE_LOOP('',(#6753,#6754,#6755,#6756));
#1201=EDGE_LOOP('',(#6757,#6758,#6759,#6760));
#1202=EDGE_LOOP('',(#6761,#6762,#6763,#6764));
#1203=EDGE_LOOP('',(#6765,#6766,#6767,#6768));
#1204=EDGE_LOOP('',(#6769,#6770,#6771,#6772));
#1205=EDGE_LOOP('',(#6773,#6774,#6775,#6776));
#1206=EDGE_LOOP('',(#6777,#6778,#6779,#6780));
#1207=EDGE_LOOP('',(#6781,#6782,#6783,#6784));
#1208=EDGE_LOOP('',(#6785,#6786,#6787,#6788));
#1209=EDGE_LOOP('',(#6789,#6790,#6791,#6792));
#1210=EDGE_LOOP('',(#6793,#6794,#6795,#6796));
#1211=EDGE_LOOP('',(#6797,#6798,#6799,#6800,#6801,#6802));
#1212=EDGE_LOOP('',(#6803,#6804,#6805,#6806));
#1213=EDGE_LOOP('',(#6807,#6808,#6809,#6810,#6811,#6812));
#1214=EDGE_LOOP('',(#6813,#6814,#6815,#6816));
#1215=EDGE_LOOP('',(#6817,#6818,#6819,#6820));
#1216=EDGE_LOOP('',(#6821));
#1217=EDGE_LOOP('',(#6822));
#1218=EDGE_LOOP('',(#6823));
#1219=EDGE_LOOP('',(#6824));
#1220=EDGE_LOOP('',(#6825,#6826,#6827,#6828));
#1221=EDGE_LOOP('',(#6829,#6830,#6831,#6832));
#1222=EDGE_LOOP('',(#6833,#6834,#6835,#6836));
#1223=EDGE_LOOP('',(#6837,#6838,#6839,#6840));
#1224=EDGE_LOOP('',(#6841,#6842,#6843,#6844));
#1225=EDGE_LOOP('',(#6845,#6846,#6847,#6848));
#1226=EDGE_LOOP('',(#6849,#6850,#6851,#6852));
#1227=EDGE_LOOP('',(#6853,#6854,#6855,#6856));
#1228=EDGE_LOOP('',(#6857));
#1229=EDGE_LOOP('',(#6858));
#1230=EDGE_LOOP('',(#6859));
#1231=EDGE_LOOP('',(#6860));
#1232=EDGE_LOOP('',(#6861,#6862,#6863,#6864));
#1233=EDGE_LOOP('',(#6865,#6866,#6867,#6868));
#1234=EDGE_LOOP('',(#6869,#6870,#6871,#6872));
#1235=EDGE_LOOP('',(#6873,#6874,#6875,#6876));
#1236=EDGE_LOOP('',(#6877,#6878,#6879,#6880));
#1237=EDGE_LOOP('',(#6881,#6882,#6883,#6884));
#1238=EDGE_LOOP('',(#6885,#6886,#6887,#6888));
#1239=EDGE_LOOP('',(#6889,#6890,#6891,#6892));
#1240=EDGE_LOOP('',(#6893,#6894,#6895,#6896));
#1241=EDGE_LOOP('',(#6897,#6898,#6899,#6900));
#1242=EDGE_LOOP('',(#6901,#6902,#6903,#6904));
#1243=EDGE_LOOP('',(#6905,#6906,#6907,#6908));
#1244=EDGE_LOOP('',(#6909,#6910,#6911,#6912));
#1245=EDGE_LOOP('',(#6913,#6914,#6915,#6916));
#1246=EDGE_LOOP('',(#6917,#6918,#6919,#6920));
#1247=EDGE_LOOP('',(#6921,#6922,#6923,#6924));
#1248=EDGE_LOOP('',(#6925,#6926,#6927,#6928));
#1249=EDGE_LOOP('',(#6929,#6930,#6931,#6932));
#1250=EDGE_LOOP('',(#6933,#6934,#6935,#6936));
#1251=EDGE_LOOP('',(#6937,#6938,#6939,#6940));
#1252=EDGE_LOOP('',(#6941,#6942,#6943,#6944,#6945,#6946,#6947,#6948));
#1253=EDGE_LOOP('',(#6949,#6950,#6951,#6952,#6953,#6954,#6955,#6956,#6957,
#6958,#6959,#6960,#6961,#6962,#6963,#6964,#6965,#6966,#6967,#6968,#6969,
#6970,#6971,#6972));
#1254=EDGE_LOOP('',(#6973,#6974,#6975,#6976));
#1255=EDGE_LOOP('',(#6977,#6978,#6979,#6980,#6981,#6982,#6983,#6984,#6985,
#6986,#6987,#6988,#6989,#6990,#6991,#6992,#6993,#6994,#6995,#6996,#6997,
#6998,#6999,#7000,#7001));
#1256=EDGE_LOOP('',(#7002,#7003,#7004,#7005));
#1257=EDGE_LOOP('',(#7006,#7007,#7008,#7009));
#1258=EDGE_LOOP('',(#7010,#7011,#7012,#7013));
#1259=EDGE_LOOP('',(#7014,#7015,#7016,#7017));
#1260=EDGE_LOOP('',(#7018,#7019,#7020,#7021));
#1261=EDGE_LOOP('',(#7022,#7023,#7024,#7025));
#1262=EDGE_LOOP('',(#7026,#7027,#7028,#7029));
#1263=EDGE_LOOP('',(#7030,#7031,#7032,#7033,#7034,#7035));
#1264=EDGE_LOOP('',(#7036));
#1265=EDGE_LOOP('',(#7037,#7038,#7039,#7040));
#1266=EDGE_LOOP('',(#7041,#7042,#7043,#7044));
#1267=EDGE_LOOP('',(#7045));
#1268=EDGE_LOOP('',(#7046,#7047,#7048,#7049,#7050,#7051));
#1269=EDGE_LOOP('',(#7052));
#1270=EDGE_LOOP('',(#7053,#7054,#7055,#7056));
#1271=EDGE_LOOP('',(#7057,#7058,#7059,#7060,#7061,#7062,#7063,#7064));
#1272=EDGE_LOOP('',(#7065));
#1273=EDGE_LOOP('',(#7066));
#1274=EDGE_LOOP('',(#7067,#7068,#7069,#7070));
#1275=EDGE_LOOP('',(#7071,#7072,#7073,#7074));
#1276=EDGE_LOOP('',(#7075,#7076,#7077,#7078));
#1277=EDGE_LOOP('',(#7079,#7080,#7081,#7082));
#1278=EDGE_LOOP('',(#7083,#7084,#7085,#7086));
#1279=EDGE_LOOP('',(#7087));
#1280=EDGE_LOOP('',(#7088,#7089,#7090,#7091));
#1281=EDGE_LOOP('',(#7092));
#1282=EDGE_LOOP('',(#7093,#7094,#7095,#7096));
#1283=EDGE_LOOP('',(#7097,#7098,#7099,#7100));
#1284=EDGE_LOOP('',(#7101,#7102,#7103,#7104));
#1285=EDGE_LOOP('',(#7105));
#1286=EDGE_LOOP('',(#7106,#7107,#7108,#7109));
#1287=EDGE_LOOP('',(#7110));
#1288=EDGE_LOOP('',(#7111,#7112,#7113,#7114));
#1289=EDGE_LOOP('',(#7115,#7116,#7117,#7118,#7119,#7120,#7121,#7122));
#1290=EDGE_LOOP('',(#7123));
#1291=EDGE_LOOP('',(#7124));
#1292=EDGE_LOOP('',(#7125,#7126,#7127,#7128));
#1293=EDGE_LOOP('',(#7129));
#1294=EDGE_LOOP('',(#7130));
#1295=EDGE_LOOP('',(#7131));
#1296=EDGE_LOOP('',(#7132));
#1297=EDGE_LOOP('',(#7133,#7134,#7135,#7136));
#1298=EDGE_LOOP('',(#7137));
#1299=EDGE_LOOP('',(#7138));
#1300=EDGE_LOOP('',(#7139,#7140,#7141,#7142));
#1301=EDGE_LOOP('',(#7143));
#1302=EDGE_LOOP('',(#7144,#7145,#7146,#7147));
#1303=EDGE_LOOP('',(#7148));
#1304=EDGE_LOOP('',(#7149,#7150,#7151,#7152));
#1305=EDGE_LOOP('',(#7153,#7154,#7155,#7156));
#1306=EDGE_LOOP('',(#7157,#7158,#7159,#7160));
#1307=EDGE_LOOP('',(#7161,#7162,#7163,#7164));
#1308=EDGE_LOOP('',(#7165,#7166,#7167,#7168));
#1309=EDGE_LOOP('',(#7169,#7170,#7171,#7172));
#1310=EDGE_LOOP('',(#7173,#7174,#7175,#7176));
#1311=EDGE_LOOP('',(#7177,#7178,#7179,#7180));
#1312=EDGE_LOOP('',(#7181,#7182,#7183,#7184,#7185,#7186,#7187,#7188));
#1313=EDGE_LOOP('',(#7189));
#1314=EDGE_LOOP('',(#7190));
#1315=EDGE_LOOP('',(#7191,#7192,#7193,#7194));
#1316=EDGE_LOOP('',(#7195,#7196,#7197,#7198));
#1317=EDGE_LOOP('',(#7199,#7200,#7201,#7202));
#1318=EDGE_LOOP('',(#7203,#7204,#7205,#7206));
#1319=EDGE_LOOP('',(#7207));
#1320=EDGE_LOOP('',(#7208,#7209,#7210,#7211));
#1321=EDGE_LOOP('',(#7212,#7213,#7214,#7215));
#1322=EDGE_LOOP('',(#7216,#7217,#7218,#7219));
#1323=EDGE_LOOP('',(#7220));
#1324=EDGE_LOOP('',(#7221,#7222,#7223,#7224));
#1325=EDGE_LOOP('',(#7225,#7226,#7227,#7228));
#1326=EDGE_LOOP('',(#7229,#7230,#7231,#7232,#7233,#7234,#7235,#7236));
#1327=EDGE_LOOP('',(#7237));
#1328=EDGE_LOOP('',(#7238));
#1329=EDGE_LOOP('',(#7239,#7240,#7241,#7242));
#1330=EDGE_LOOP('',(#7243,#7244,#7245,#7246));
#1331=EDGE_LOOP('',(#7247));
#1332=EDGE_LOOP('',(#7248));
#1333=EDGE_LOOP('',(#7249));
#1334=EDGE_LOOP('',(#7250));
#1335=EDGE_LOOP('',(#7251,#7252,#7253,#7254));
#1336=EDGE_LOOP('',(#7255,#7256,#7257,#7258));
#1337=EDGE_LOOP('',(#7259,#7260,#7261,#7262));
#1338=EDGE_LOOP('',(#7263,#7264,#7265,#7266));
#1339=EDGE_LOOP('',(#7267,#7268,#7269,#7270));
#1340=EDGE_LOOP('',(#7271,#7272,#7273,#7274));
#1341=EDGE_LOOP('',(#7275,#7276,#7277,#7278));
#1342=EDGE_LOOP('',(#7279,#7280,#7281,#7282));
#1343=EDGE_LOOP('',(#7283,#7284,#7285,#7286));
#1344=EDGE_LOOP('',(#7287,#7288,#7289,#7290));
#1345=EDGE_LOOP('',(#7291,#7292,#7293,#7294));
#1346=EDGE_LOOP('',(#7295,#7296,#7297,#7298));
#1347=EDGE_LOOP('',(#7299,#7300,#7301,#7302));
#1348=EDGE_LOOP('',(#7303,#7304,#7305,#7306));
#1349=EDGE_LOOP('',(#7307,#7308,#7309,#7310));
#1350=EDGE_LOOP('',(#7311,#7312,#7313,#7314));
#1351=EDGE_LOOP('',(#7315,#7316,#7317,#7318));
#1352=EDGE_LOOP('',(#7319,#7320,#7321,#7322));
#1353=EDGE_LOOP('',(#7323,#7324,#7325,#7326));
#1354=EDGE_LOOP('',(#7327,#7328,#7329,#7330));
#1355=EDGE_LOOP('',(#7331,#7332,#7333,#7334));
#1356=EDGE_LOOP('',(#7335,#7336,#7337,#7338));
#1357=EDGE_LOOP('',(#7339,#7340,#7341,#7342));
#1358=EDGE_LOOP('',(#7343,#7344,#7345,#7346));
#1359=EDGE_LOOP('',(#7347,#7348,#7349,#7350));
#1360=EDGE_LOOP('',(#7351,#7352,#7353,#7354));
#1361=EDGE_LOOP('',(#7355,#7356,#7357,#7358));
#1362=EDGE_LOOP('',(#7359,#7360,#7361,#7362));
#1363=EDGE_LOOP('',(#7363,#7364,#7365,#7366));
#1364=EDGE_LOOP('',(#7367,#7368,#7369,#7370));
#1365=EDGE_LOOP('',(#7371,#7372,#7373,#7374));
#1366=EDGE_LOOP('',(#7375,#7376,#7377,#7378));
#1367=EDGE_LOOP('',(#7379,#7380,#7381,#7382));
#1368=EDGE_LOOP('',(#7383,#7384,#7385,#7386));
#1369=EDGE_LOOP('',(#7387,#7388,#7389,#7390));
#1370=EDGE_LOOP('',(#7391,#7392,#7393,#7394));
#1371=EDGE_LOOP('',(#7395,#7396,#7397,#7398));
#1372=EDGE_LOOP('',(#7399,#7400,#7401,#7402));
#1373=EDGE_LOOP('',(#7403,#7404,#7405,#7406,#7407,#7408,#7409,#7410));
#1374=EDGE_LOOP('',(#7411,#7412,#7413,#7414,#7415,#7416,#7417,#7418,#7419,
#7420,#7421,#7422,#7423,#7424,#7425,#7426,#7427,#7428,#7429,#7430,#7431,
#7432,#7433,#7434,#7435,#7436,#7437,#7438,#7439,#7440,#7441,#7442,#7443,
#7444,#7445,#7446,#7447,#7448,#7449,#7450,#7451,#7452));
#1375=EDGE_LOOP('',(#7453,#7454,#7455,#7456));
#1376=EDGE_LOOP('',(#7457,#7458,#7459,#7460,#7461,#7462,#7463,#7464,#7465,
#7466,#7467,#7468,#7469,#7470,#7471,#7472,#7473,#7474,#7475,#7476,#7477,
#7478,#7479,#7480,#7481,#7482,#7483,#7484,#7485,#7486,#7487,#7488,#7489,
#7490,#7491,#7492,#7493,#7494,#7495,#7496,#7497,#7498,#7499));
#1377=EDGE_LOOP('',(#7500,#7501,#7502,#7503));
#1378=EDGE_LOOP('',(#7504,#7505,#7506,#7507));
#1379=EDGE_LOOP('',(#7508,#7509,#7510,#7511));
#1380=EDGE_LOOP('',(#7512,#7513,#7514,#7515));
#1381=EDGE_LOOP('',(#7516,#7517,#7518,#7519));
#1382=EDGE_LOOP('',(#7520,#7521,#7522,#7523));
#1383=EDGE_LOOP('',(#7524,#7525,#7526,#7527));
#1384=EDGE_LOOP('',(#7528,#7529,#7530,#7531,#7532,#7533));
#1385=EDGE_LOOP('',(#7534));
#1386=EDGE_LOOP('',(#7535,#7536,#7537,#7538));
#1387=EDGE_LOOP('',(#7539,#7540,#7541,#7542));
#1388=EDGE_LOOP('',(#7543));
#1389=EDGE_LOOP('',(#7544,#7545,#7546,#7547,#7548,#7549));
#1390=EDGE_LOOP('',(#7550));
#1391=EDGE_LOOP('',(#7551,#7552,#7553,#7554));
#1392=EDGE_LOOP('',(#7555,#7556,#7557,#7558));
#1393=EDGE_LOOP('',(#7559,#7560,#7561,#7562));
#1394=EDGE_LOOP('',(#7563,#7564,#7565,#7566));
#1395=EDGE_LOOP('',(#7567,#7568,#7569,#7570));
#1396=EDGE_LOOP('',(#7571,#7572,#7573,#7574));
#1397=EDGE_LOOP('',(#7575,#7576,#7577,#7578));
#1398=EDGE_LOOP('',(#7579,#7580,#7581,#7582));
#1399=EDGE_LOOP('',(#7583,#7584,#7585,#7586));
#1400=EDGE_LOOP('',(#7587,#7588,#7589,#7590));
#1401=EDGE_LOOP('',(#7591,#7592,#7593,#7594));
#1402=EDGE_LOOP('',(#7595,#7596,#7597,#7598));
#1403=EDGE_LOOP('',(#7599,#7600,#7601,#7602));
#1404=EDGE_LOOP('',(#7603,#7604,#7605,#7606));
#1405=EDGE_LOOP('',(#7607,#7608,#7609,#7610));
#1406=EDGE_LOOP('',(#7611,#7612,#7613,#7614));
#1407=EDGE_LOOP('',(#7615,#7616,#7617,#7618));
#1408=EDGE_LOOP('',(#7619,#7620,#7621,#7622));
#1409=EDGE_LOOP('',(#7623,#7624,#7625,#7626));
#1410=EDGE_LOOP('',(#7627,#7628,#7629,#7630));
#1411=EDGE_LOOP('',(#7631,#7632,#7633,#7634));
#1412=EDGE_LOOP('',(#7635,#7636,#7637,#7638));
#1413=EDGE_LOOP('',(#7639,#7640,#7641,#7642,#7643,#7644,#7645,#7646));
#1414=EDGE_LOOP('',(#7647,#7648,#7649,#7650,#7651,#7652,#7653,#7654,#7655,
#7656,#7657,#7658,#7659,#7660,#7661,#7662,#7663,#7664,#7665,#7666,#7667,
#7668,#7669,#7670,#7671,#7672));
#1415=EDGE_LOOP('',(#7673,#7674,#7675,#7676));
#1416=EDGE_LOOP('',(#7677,#7678,#7679,#7680,#7681,#7682,#7683,#7684,#7685,
#7686,#7687,#7688,#7689,#7690,#7691,#7692,#7693,#7694,#7695,#7696,#7697,
#7698,#7699,#7700,#7701,#7702,#7703));
#1417=EDGE_LOOP('',(#7704,#7705,#7706,#7707));
#1418=EDGE_LOOP('',(#7708,#7709,#7710,#7711));
#1419=EDGE_LOOP('',(#7712,#7713,#7714,#7715));
#1420=EDGE_LOOP('',(#7716,#7717,#7718,#7719));
#1421=EDGE_LOOP('',(#7720,#7721,#7722,#7723));
#1422=EDGE_LOOP('',(#7724,#7725,#7726,#7727));
#1423=EDGE_LOOP('',(#7728,#7729,#7730,#7731));
#1424=EDGE_LOOP('',(#7732,#7733,#7734,#7735,#7736,#7737));
#1425=EDGE_LOOP('',(#7738));
#1426=EDGE_LOOP('',(#7739,#7740,#7741,#7742));
#1427=EDGE_LOOP('',(#7743,#7744,#7745,#7746));
#1428=EDGE_LOOP('',(#7747));
#1429=EDGE_LOOP('',(#7748,#7749,#7750,#7751,#7752,#7753));
#1430=EDGE_LOOP('',(#7754));
#1431=EDGE_LOOP('',(#7755,#7756,#7757,#7758));
#1432=EDGE_LOOP('',(#7759,#7760,#7761,#7762));
#1433=EDGE_LOOP('',(#7763));
#1434=EDGE_LOOP('',(#7764));
#1435=EDGE_LOOP('',(#7765));
#1436=EDGE_LOOP('',(#7766));
#1437=EDGE_LOOP('',(#7767,#7768,#7769,#7770));
#1438=EDGE_LOOP('',(#7771,#7772,#7773,#7774));
#1439=EDGE_LOOP('',(#7775,#7776,#7777,#7778));
#1440=EDGE_LOOP('',(#7779,#7780,#7781,#7782));
#1441=EDGE_LOOP('',(#7783,#7784,#7785,#7786));
#1442=EDGE_LOOP('',(#7787,#7788,#7789,#7790));
#1443=EDGE_LOOP('',(#7791,#7792,#7793,#7794));
#1444=EDGE_LOOP('',(#7795,#7796,#7797,#7798));
#1445=EDGE_LOOP('',(#7799,#7800,#7801,#7802));
#1446=EDGE_LOOP('',(#7803,#7804,#7805,#7806));
#1447=EDGE_LOOP('',(#7807,#7808,#7809,#7810));
#1448=EDGE_LOOP('',(#7811,#7812,#7813,#7814,#7815,#7816,#7817,#7818,#7819,
#7820,#7821,#7822,#7823,#7824));
#1449=EDGE_LOOP('',(#7825,#7826,#7827,#7828,#7829,#7830,#7831,#7832,#7833,
#7834,#7835,#7836,#7837,#7838));
#1450=EDGE_LOOP('',(#7839,#7840,#7841,#7842,#7843,#7844));
#1451=EDGE_LOOP('',(#7845,#7846,#7847,#7848));
#1452=EDGE_LOOP('',(#7849,#7850,#7851,#7852));
#1453=EDGE_LOOP('',(#7853,#7854,#7855,#7856));
#1454=EDGE_LOOP('',(#7857,#7858,#7859,#7860));
#1455=EDGE_LOOP('',(#7861,#7862,#7863,#7864));
#1456=EDGE_LOOP('',(#7865,#7866,#7867,#7868));
#1457=EDGE_LOOP('',(#7869,#7870,#7871,#7872));
#1458=EDGE_LOOP('',(#7873,#7874,#7875,#7876));
#1459=EDGE_LOOP('',(#7877,#7878,#7879,#7880,#7881,#7882));
#1460=EDGE_LOOP('',(#7883,#7884,#7885,#7886));
#1461=CIRCLE('',#8895,2.5175);
#1462=CIRCLE('',#8896,2.5175);
#1463=CIRCLE('',#8897,2.5175);
#1464=CIRCLE('',#8914,2.5175);
#1465=CIRCLE('',#8916,3.07349999999999);
#1466=CIRCLE('',#8933,3.0735);
#1467=CIRCLE('',#8935,2.5175);
#1468=CIRCLE('',#8936,2.5175);
#1469=CIRCLE('',#8937,2.5175);
#1470=CIRCLE('',#8954,2.5175);
#1471=CIRCLE('',#8956,3.07349999999999);
#1472=CIRCLE('',#8973,3.0735);
#1473=CIRCLE('',#8975,2.5175);
#1474=CIRCLE('',#8976,2.5175);
#1475=CIRCLE('',#8977,2.5175);
#1476=CIRCLE('',#8994,2.5175);
#1477=CIRCLE('',#8996,3.07349999999996);
#1478=CIRCLE('',#9013,3.07349999999996);
#1479=CIRCLE('',#9015,2.5175);
#1480=CIRCLE('',#9016,2.5175);
#1481=CIRCLE('',#9017,2.5175);
#1482=CIRCLE('',#9034,2.5175);
#1483=CIRCLE('',#9036,3.07350000000003);
#1484=CIRCLE('',#9053,3.07350000000003);
#1485=CIRCLE('',#9082,4.5);
#1486=CIRCLE('',#9083,4.5);
#1487=CIRCLE('',#9085,3.5);
#1488=CIRCLE('',#9086,3.5);
#1489=CIRCLE('',#9088,3.5);
#1490=CIRCLE('',#9089,3.5);
#1491=CIRCLE('',#9091,3.5);
#1492=CIRCLE('',#9092,3.5);
#1493=CIRCLE('',#9094,3.5);
#1494=CIRCLE('',#9095,3.5);
#1495=CIRCLE('',#9115,1.666);
#1496=CIRCLE('',#9116,1.666);
#1497=CIRCLE('',#9131,1.666);
#1498=CIRCLE('',#9133,2.05475);
#1499=CIRCLE('',#9149,2.05475);
#1500=CIRCLE('',#9160,3.);
#1501=CIRCLE('',#9161,3.);
#1502=CIRCLE('',#9163,4.);
#1503=CIRCLE('',#9165,4.);
#1504=CIRCLE('',#9167,4.);
#1505=CIRCLE('',#9176,10.);
#1506=CIRCLE('',#9177,4.);
#1507=CIRCLE('',#9179,10.);
#1508=CIRCLE('',#9198,4.);
#1509=CIRCLE('',#9199,4.);
#1510=CIRCLE('',#9201,8.);
#1511=CIRCLE('',#9202,8.);
#1512=CIRCLE('',#9209,6.);
#1513=CIRCLE('',#9210,3.);
#1514=CIRCLE('',#9212,3.);
#1515=CIRCLE('',#9214,6.);
#1516=CIRCLE('',#9218,2.5);
#1517=CIRCLE('',#9219,2.5);
#1518=CIRCLE('',#9221,4.5);
#1519=CIRCLE('',#9222,4.5);
#1520=CIRCLE('',#9227,1.954);
#1521=CIRCLE('',#9238,1.5555);
#1522=CIRCLE('',#9249,1.954);
#1523=CIRCLE('',#9250,1.);
#1524=CIRCLE('',#9252,1.5555);
#1525=CIRCLE('',#9262,3.5);
#1526=CIRCLE('',#9264,3.5);
#1527=CIRCLE('',#9270,3.5);
#1528=CIRCLE('',#9271,3.5);
#1529=CIRCLE('',#9273,3.5);
#1530=CIRCLE('',#9275,3.5);
#1531=CIRCLE('',#9277,5.);
#1532=CIRCLE('',#9278,5.);
#1533=CIRCLE('',#9280,2.);
#1534=CIRCLE('',#9281,2.);
#1535=CIRCLE('',#9284,5.);
#1536=CIRCLE('',#9285,2.);
#1537=CIRCLE('',#9287,2.);
#1538=CIRCLE('',#9289,5.);
#1539=CIRCLE('',#9296,1.5);
#1540=CIRCLE('',#9297,1.5);
#1541=CIRCLE('',#9299,2.);
#1542=CIRCLE('',#9301,2.);
#1543=CIRCLE('',#9303,2.);
#1544=CIRCLE('',#9305,4.);
#1545=CIRCLE('',#9306,2.);
#1546=CIRCLE('',#9308,4.);
#1547=CIRCLE('',#9316,4.);
#1548=CIRCLE('',#9317,1.5);
#1549=CIRCLE('',#9319,1.5);
#1550=CIRCLE('',#9321,4.);
#1551=CIRCLE('',#9327,3.5);
#1552=CIRCLE('',#9328,3.5);
#1553=CIRCLE('',#9331,3.5);
#1554=CIRCLE('',#9333,3.5);
#1555=CIRCLE('',#9335,5.);
#1556=CIRCLE('',#9336,2.);
#1557=CIRCLE('',#9338,2.);
#1558=CIRCLE('',#9340,5.);
#1559=CIRCLE('',#9347,3.5);
#1560=CIRCLE('',#9348,3.5);
#1561=CIRCLE('',#9350,5.);
#1562=CIRCLE('',#9351,5.);
#1563=CIRCLE('',#9356,2.942);
#1564=CIRCLE('',#9376,2.37175);
#1565=CIRCLE('',#9396,2.942);
#1566=CIRCLE('',#9397,2.);
#1567=CIRCLE('',#9399,2.37175);
#1568=CIRCLE('',#9409,5.);
#1569=CIRCLE('',#9411,5.);
#1570=CIRCLE('',#9416,2.942);
#1571=CIRCLE('',#9428,2.37175);
#1572=CIRCLE('',#9440,2.942);
#1573=CIRCLE('',#9441,2.);
#1574=CIRCLE('',#9443,2.37175);
#1575=CIRCLE('',#9453,5.);
#1576=CIRCLE('',#9455,5.);
#1577=CIRCLE('',#9460,3.5);
#1578=CIRCLE('',#9461,3.5);
#1579=CIRCLE('',#9463,7.);
#1580=CIRCLE('',#9464,7.);
#1581=CIRCLE('',#9469,2.5175);
#1582=CIRCLE('',#9474,2.5175);
#1583=CIRCLE('',#9476,3.0735);
#1584=CIRCLE('',#9481,3.0735);
#1585=B_SPLINE_CURVE_WITH_KNOTS('',3,(#11356,#11357,#11358,#11359),
 .UNSPECIFIED.,.F.,.F.,(4,4),(108.12371336303,108.831095115081),
 .UNSPECIFIED.);
#1586=B_SPLINE_CURVE_WITH_KNOTS('',3,(#11367,#11368,#11369,#11370,#11371,
#11372,#11373,#11374,#11375,#11376),.UNSPECIFIED.,.F.,.F.,(4,3,3,4),(-106.814150222053,
-105.835743873382,-104.837293459482,-104.379939320515),.UNSPECIFIED.);
#1587=B_SPLINE_CURVE_WITH_KNOTS('',3,(#11381,#11382,#11383,#11384,#11385,
#11386,#11387,#11388,#11389,#11390,#11391,#11392,#11393,#11394,#11395,#11396,
#11397,#11398,#11399,#11400,#11401,#11402),.UNSPECIFIED.,.F.,.F.,(4,3,3,
3,3,3,3,4),(101.84052805585,102.840392631682,103.838843045582,104.837293459482,
105.835743873382,106.834194287282,107.832644701182,108.12371336303),
 .UNSPECIFIED.);
#1588=B_SPLINE_CURVE_WITH_KNOTS('',3,(#11403,#11404,#11405,#11406,#11407,
#11408,#11409,#11410,#11411,#11412,#11413,#11414,#11415,#11416,#11417,#11418,
#11419,#11420,#11421,#11422,#11423,#11424),.UNSPECIFIED.,.F.,.F.,(4,3,3,
3,3,3,3,4),(-104.379939320515,-103.838843045582,-102.840392631682,-101.841942217783,
-100.843491803883,-99.8450413899829,-98.8465909760831,-98.096754013335),
 .UNSPECIFIED.);
#1589=B_SPLINE_CURVE_WITH_KNOTS('',3,(#11429,#11430,#11431,#11432,#11433,
#11434,#11435,#11436,#11437,#11438,#11439,#11440,#11441,#11442,#11443,#11444,
#11445,#11446,#11447,#11448,#11449,#11450),.UNSPECIFIED.,.F.,.F.,(4,3,3,
3,3,3,3,4),(95.5573427486709,95.8512397343836,96.8496901482835,97.8481405621833,
98.8465909760831,99.845041389983,100.843491803883,101.84052805585),
 .UNSPECIFIED.);
#1590=B_SPLINE_CURVE_WITH_KNOTS('',3,(#11451,#11452,#11453,#11454,#11455,
#11456,#11457,#11458,#11459,#11460,#11461,#11462,#11463,#11464,#11465,#11466,
#11467,#11468,#11469,#11470,#11471,#11472,#11473,#11474,#11475),
 .UNSPECIFIED.,.F.,.F.,(4,3,3,3,3,3,3,3,4),(-98.096754013335,-97.8481405621833,
-96.8496901482834,-95.8512397343836,-94.8527893204838,-93.854338906584,
-92.8558884926841,-91.8574380787843,-91.8135687061554),.UNSPECIFIED.);
#1591=B_SPLINE_CURVE_WITH_KNOTS('',3,(#11480,#11481,#11482,#11483,#11484,
#11485,#11486,#11487,#11488,#11489,#11490,#11491,#11492,#11493,#11494,#11495,
#11496,#11497,#11498,#11499,#11500,#11501),.UNSPECIFIED.,.F.,.F.,(4,3,3,
3,3,3,3,4),(89.2741574414913,89.8605372509847,90.8589876648845,91.8574380787843,
92.8558884926841,93.854338906584,94.8527893204838,95.5573427486709),
 .UNSPECIFIED.);
#1592=B_SPLINE_CURVE_WITH_KNOTS('',3,(#11502,#11503,#11504,#11505,#11506,
#11507,#11508,#11509,#11510,#11511,#11512,#11513,#11514,#11515,#11516,#11517,
#11518,#11519,#11520,#11521,#11522,#11523),.UNSPECIFIED.,.F.,.F.,(4,3,3,
3,3,3,3,4),(-91.8135687061554,-90.8589876648845,-89.8605372509847,-88.8620868370848,
-87.863636423185,-86.8651860092852,-85.8667355953853,-85.5303833989758),
 .UNSPECIFIED.);
#1593=B_SPLINE_CURVE_WITH_KNOTS('',3,(#11528,#11529,#11530,#11531,#11532,
#11533,#11534,#11535,#11536,#11537,#11538,#11539,#11540,#11541,#11542,#11543,
#11544,#11545,#11546,#11547,#11548,#11549),.UNSPECIFIED.,.F.,.F.,(4,3,3,
3,3,3,3,4),(82.9909721343117,83.8698347675857,84.8682851814855,85.8667355953854,
86.8651860092852,87.863636423185,88.8620868370848,89.2741574414913),
 .UNSPECIFIED.);
#1594=B_SPLINE_CURVE_WITH_KNOTS('',3,(#11550,#11551,#11552,#11553,#11554,
#11555,#11556,#11557,#11558,#11559,#11560,#11561,#11562,#11563,#11564,#11565,
#11566,#11567,#11568,#11569,#11570,#11571),.UNSPECIFIED.,.F.,.F.,(4,3,3,
3,3,3,3,4),(-85.5303833989758,-84.8682851814855,-83.8698347675857,-82.8713843536859,
-81.872933939786,-80.8744835258862,-79.8760331119863,-79.2471980917962),
 .UNSPECIFIED.);
#1595=B_SPLINE_CURVE_WITH_KNOTS('',3,(#11576,#11577,#11578,#11579,#11580,
#11581,#11582,#11583,#11584,#11585,#11586,#11587,#11588,#11589,#11590,#11591,
#11592,#11593,#11594,#11595,#11596,#11597,#11598,#11599,#11600),
 .UNSPECIFIED.,.F.,.F.,(4,3,3,3,3,3,3,3,4),(76.7077868271321,76.8806818702869,
77.8791322841867,78.8775826980865,79.8760331119864,80.8744835258862,81.872933939786,
82.8713843536859,82.9909721343117),.UNSPECIFIED.);
#1596=B_SPLINE_CURVE_WITH_KNOTS('',3,(#11601,#11602,#11603,#11604,#11605,
#11606,#11607,#11608,#11609,#11610,#11611,#11612,#11613,#11614,#11615,#11616,
#11617,#11618,#11619,#11620,#11621,#11622),.UNSPECIFIED.,.F.,.F.,(4,3,3,
3,3,3,3,4),(-79.2471980917962,-78.8775826980865,-77.8791322841867,-76.8806818702868,
-75.882231456387,-74.8837810424872,-73.8853306285873,-72.9640127846166),
 .UNSPECIFIED.);
#1597=B_SPLINE_CURVE_WITH_KNOTS('',3,(#11627,#11628,#11629,#11630,#11631,
#11632,#11633,#11634,#11635,#11636,#11637,#11638,#11639,#11640,#11641,#11642,
#11643,#11644,#11645,#11646,#11647,#11648),.UNSPECIFIED.,.F.,.F.,(4,3,3,
3,3,3,3,4),(70.4246015199525,70.8899793868879,71.8884298007877,72.8868802146876,
73.8853306285874,74.8837810424872,75.882231456387,76.7077868271321),
 .UNSPECIFIED.);
#1598=B_SPLINE_CURVE_WITH_KNOTS('',3,(#11649,#11650,#11651,#11652,#11653,
#11654,#11655,#11656,#11657,#11658,#11659,#11660,#11661,#11662,#11663,#11664,
#11665,#11666,#11667,#11668,#11669,#11670,#11671,#11672,#11673),
 .UNSPECIFIED.,.F.,.F.,(4,3,3,3,3,3,3,3,4),(-72.9640127846166,-72.8868802146875,
-71.8884298007877,-70.8899793868879,-69.891528972988,-68.8930785590882,
-67.8946281451884,-66.8961777312885,-66.680827477437),.UNSPECIFIED.);
#1599=B_SPLINE_CURVE_WITH_KNOTS('',3,(#11678,#11679,#11680,#11681,#11682,
#11683,#11684,#11685,#11686,#11687,#11688,#11689,#11690,#11691,#11692,#11693,
#11694,#11695,#11696,#11697,#11698,#11699),.UNSPECIFIED.,.F.,.F.,(4,3,3,
3,3,3,3,4),(64.1414162127729,64.8992769034889,65.8977273173887,66.8961777312886,
67.8946281451884,68.8930785590882,69.8915289729881,70.4246015199525),
 .UNSPECIFIED.);
#1600=B_SPLINE_CURVE_WITH_KNOTS('',3,(#11700,#11701,#11702,#11703,#11704,
#11705,#11706,#11707,#11708,#11709,#11710,#11711,#11712,#11713,#11714,#11715,
#11716,#11717,#11718,#11719,#11720,#11721),.UNSPECIFIED.,.F.,.F.,(4,3,3,
3,3,3,3,4),(-66.680827477437,-65.8977273173887,-64.8992769034889,-63.9008264895891,
-62.9023760756892,-61.9039256617894,-60.9054752478896,-60.3976421702574),
 .UNSPECIFIED.);
#1601=B_SPLINE_CURVE_WITH_KNOTS('',3,(#11726,#11727,#11728,#11729,#11730,
#11731,#11732,#11733,#11734,#11735,#11736,#11737,#11738,#11739,#11740,#11741,
#11742,#11743,#11744,#11745,#11746,#11747,#11748,#11749,#11750),
 .UNSPECIFIED.,.F.,.F.,(4,3,3,3,3,3,3,3,4),(57.8582309055933,57.9101240061901,
58.9085744200899,59.9070248339898,60.9054752478896,61.9039256617894,62.9023760756893,
63.9008264895891,64.1414162127729),.UNSPECIFIED.);
#1602=B_SPLINE_CURVE_WITH_KNOTS('',3,(#11751,#11752,#11753,#11754,#11755,
#11756,#11757,#11758,#11759,#11760,#11761,#11762,#11763,#11764,#11765,#11766,
#11767,#11768,#11769,#11770,#11771,#11772),.UNSPECIFIED.,.F.,.F.,(4,3,3,
3,3,3,3,4),(-60.3976421702574,-59.9070248339898,-58.9085744200899,-57.9101240061901,
-56.9116735922903,-55.9132231783904,-54.9147727644906,-54.1144568630778),
 .UNSPECIFIED.);
#1603=B_SPLINE_CURVE_WITH_KNOTS('',3,(#11777,#11778,#11779,#11780,#11781,
#11782,#11783,#11784,#11785,#11786,#11787,#11788,#11789,#11790,#11791,#11792,
#11793,#11794,#11795,#11796,#11797,#11798),.UNSPECIFIED.,.F.,.F.,(4,3,3,
3,3,3,3,4),(51.5750455984138,51.9194215227911,52.917871936691,53.9163223505908,
54.9147727644906,55.9132231783905,56.9116735922903,57.8582309055933),
 .UNSPECIFIED.);
#1604=B_SPLINE_CURVE_WITH_KNOTS('',3,(#11799,#11800,#11801,#11802,#11803,
#11804,#11805,#11806,#11807,#11808,#11809,#11810,#11811,#11812,#11813,#11814,
#11815,#11816,#11817,#11818,#11819,#11820,#11821,#11822,#11823),
 .UNSPECIFIED.,.F.,.F.,(4,3,3,3,3,3,3,3,4),(-54.1144568630778,-53.9163223505908,
-52.917871936691,-51.9194215227911,-50.9209711088913,-49.9225206949915,
-48.9240702810916,-47.9256198671918,-47.8312715558982),.UNSPECIFIED.);
#1605=B_SPLINE_CURVE_WITH_KNOTS('',3,(#11828,#11829,#11830,#11831,#11832,
#11833,#11834,#11835,#11836,#11837,#11838,#11839,#11840,#11841,#11842,#11843,
#11844,#11845,#11846,#11847,#11848,#11849),.UNSPECIFIED.,.F.,.F.,(4,3,3,
3,3,3,3,4),(45.2918602912342,45.9287190393922,46.927169453292,47.9256198671918,
48.9240702810916,49.9225206949915,50.9209711088913,51.5750455984138),
 .UNSPECIFIED.);
#1606=B_SPLINE_CURVE_WITH_KNOTS('',3,(#11850,#11851,#11852,#11853,#11854,
#11855,#11856,#11857,#11858,#11859,#11860,#11861,#11862,#11863,#11864,#11865,
#11866,#11867,#11868,#11869,#11870,#11871),.UNSPECIFIED.,.F.,.F.,(4,3,3,
3,3,3,3,4),(-47.8312715558982,-46.927169453292,-45.9287190393921,-44.9302686254923,
-43.9318182115925,-42.9333677976927,-41.9349173837928,-41.5480862487187),
 .UNSPECIFIED.);
#1607=B_SPLINE_CURVE_WITH_KNOTS('',3,(#11876,#11877,#11878,#11879,#11880,
#11881,#11882,#11883,#11884,#11885,#11886,#11887,#11888,#11889,#11890,#11891,
#11892,#11893,#11894,#11895,#11896,#11897),.UNSPECIFIED.,.F.,.F.,(4,3,3,
3,3,3,3,4),(39.0086749840546,39.9380165559932,40.936466969893,41.9349173837928,
42.9333677976927,43.9318182115925,44.9302686254923,45.2918602912342),
 .UNSPECIFIED.);
#1608=B_SPLINE_CURVE_WITH_KNOTS('',3,(#11898,#11899,#11900,#11901,#11902,
#11903,#11904,#11905,#11906,#11907,#11908,#11909,#11910,#11911,#11912,#11913,
#11914,#11915,#11916,#11917,#11918,#11919),.UNSPECIFIED.,.F.,.F.,(4,3,3,
3,3,3,3,4),(-41.5480862487187,-40.936466969893,-39.9380165559932,-38.9395661420933,
-37.9411157281935,-36.9426653142937,-35.9442149003939,-35.2649009415391),
 .UNSPECIFIED.);
#1609=B_SPLINE_CURVE_WITH_KNOTS('',3,(#11924,#11925,#11926,#11927,#11928,
#11929,#11930,#11931,#11932,#11933,#11934,#11935,#11936,#11937,#11938,#11939,
#11940,#11941,#11942,#11943,#11944,#11945,#11946,#11947,#11948),
 .UNSPECIFIED.,.F.,.F.,(4,3,3,3,3,3,3,3,4),(32.725489676875,32.9488636586944,
33.9473140725942,34.945764486494,35.9442149003939,36.9426653142937,37.9411157281935,
38.9395661420933,39.0086749840546),.UNSPECIFIED.);
#1610=B_SPLINE_CURVE_WITH_KNOTS('',3,(#11949,#11950,#11951,#11952,#11953,
#11954,#11955,#11956,#11957,#11958,#11959,#11960,#11961,#11962,#11963,#11964,
#11965,#11966,#11967,#11968,#11969,#11970),.UNSPECIFIED.,.F.,.F.,(4,3,3,
3,3,3,3,4),(-35.2649009415391,-34.945764486494,-33.9473140725942,-32.9488636586944,
-31.9504132447945,-30.9519628308947,-29.9535124169949,-28.9817156343595),
 .UNSPECIFIED.);
#1611=B_SPLINE_CURVE_WITH_KNOTS('',3,(#11975,#11976,#11977,#11978,#11979,
#11980,#11981,#11982,#11983,#11984,#11985,#11986,#11987,#11988,#11989,#11990,
#11991,#11992,#11993,#11994,#11995,#11996),.UNSPECIFIED.,.F.,.F.,(4,3,3,
3,3,3,3,4),(26.4423043696954,26.9581611752954,27.9566115891952,28.955062003095,
29.9535124169949,30.9519628308947,31.9504132447945,32.725489676875),
 .UNSPECIFIED.);
#1612=B_SPLINE_CURVE_WITH_KNOTS('',3,(#11997,#11998,#11999,#12000,#12001,
#12002,#12003,#12004,#12005,#12006,#12007,#12008,#12009,#12010,#12011,#12012,
#12013,#12014,#12015,#12016,#12017,#12018,#12019,#12020,#12021),
 .UNSPECIFIED.,.F.,.F.,(4,3,3,3,3,3,3,3,4),(-28.9817156343595,-28.955062003095,
-27.9566115891952,-26.9581611752954,-25.9597107613956,-24.9612603474957,
-23.9628099335959,-22.9643595196961,-22.6985303271799),.UNSPECIFIED.);
#1613=B_SPLINE_CURVE_WITH_KNOTS('',3,(#12026,#12027,#12028,#12029,#12030,
#12031,#12032,#12033,#12034,#12035,#12036,#12037,#12038,#12039,#12040,#12041,
#12042,#12043,#12044,#12045,#12046,#12047),.UNSPECIFIED.,.F.,.F.,(4,3,3,
3,3,3,3,4),(20.1591190625158,20.9674586918964,21.9659091057962,22.9643595196961,
23.9628099335959,24.9612603474957,25.9597107613956,26.4423043696954),
 .UNSPECIFIED.);
#1614=B_SPLINE_CURVE_WITH_KNOTS('',3,(#12048,#12049,#12050,#12051,#12052,
#12053,#12054,#12055,#12056,#12057,#12058,#12059,#12060,#12061,#12062,#12063,
#12064,#12065,#12066,#12067,#12068,#12069),.UNSPECIFIED.,.F.,.F.,(4,3,3,
3,3,3,3,4),(-22.6985303271799,-21.9659091057962,-20.9674586918964,-19.9690082779966,
-18.9705578640968,-17.9721074501969,-16.9736570362971,-16.4153450200003),
 .UNSPECIFIED.);
#1615=B_SPLINE_CURVE_WITH_KNOTS('',3,(#12074,#12075,#12076,#12077,#12078,
#12079,#12080,#12081,#12082,#12083,#12084,#12085,#12086,#12087,#12088,#12089,
#12090,#12091,#12092,#12093,#12094,#12095,#12096,#12097,#12098),
 .UNSPECIFIED.,.F.,.F.,(4,3,3,3,3,3,3,3,4),(13.8759337553362,13.9783057945976,
14.9767562084974,15.9752066223973,16.9736570362971,17.9721074501969,18.9705578640968,
19.9690082779966,20.1591190625158),.UNSPECIFIED.);
#1616=B_SPLINE_CURVE_WITH_KNOTS('',3,(#12099,#12100,#12101,#12102,#12103,
#12104,#12105,#12106,#12107,#12108,#12109,#12110,#12111,#12112,#12113,#12114,
#12115,#12116,#12117,#12118,#12119,#12120),.UNSPECIFIED.,.F.,.F.,(4,3,3,
3,3,3,3,4),(-16.4153450200003,-15.9752066223973,-14.9767562084974,-13.9783057945976,
-12.9798553806978,-11.9814049667979,-10.9829545528981,-10.1321597128207),
 .UNSPECIFIED.);
#1617=B_SPLINE_CURVE_WITH_KNOTS('',3,(#12126,#12127,#12128,#12129,#12130,
#12131,#12132,#12133,#12134,#12135,#12136,#12137,#12138),.UNSPECIFIED.,
 .F.,.F.,(4,3,3,3,4),(-3.84897440564113,-2.99535124169948,-1.99690082779965,
-0.998450413899827,0.),.UNSPECIFIED.);
#1618=B_SPLINE_CURVE_WITH_KNOTS('',3,(#12141,#12142,#12143,#12144,#12145,
#12146,#12147,#12148,#12149,#12150,#12151,#12152,#12153,#12154,#12155,#12156,
#12157,#12158,#12159),.UNSPECIFIED.,.F.,.F.,(4,3,3,3,3,3,4),(2.01694489302838,
2.99535124169949,3.99380165559932,4.99225206949915,5.99070248339898,6.98915289729881,
7.59274844815663),.UNSPECIFIED.);
#1619=B_SPLINE_CURVE_WITH_KNOTS('',3,(#12165,#12166,#12167,#12168,#12169,
#12170,#12171,#12172),.UNSPECIFIED.,.F.,.F.,(4,1,1,1,1,4),(116.238928182822,
116.69628232179,117.69473273569,118.693183149589,119.691633563489,120.690083977389),
 .UNSPECIFIED.);
#1620=B_SPLINE_CURVE_WITH_KNOTS('',3,(#12175,#12176,#12177,#12178,#12179,
#12180,#12181,#12182,#12183),.UNSPECIFIED.,.F.,.F.,(4,1,1,1,1,1,4),(116.238928182822,
116.240342344754,117.238792758654,118.237243172554,119.235693586454,120.234144000354,
121.212550349025),.UNSPECIFIED.);
#1621=B_SPLINE_CURVE_WITH_KNOTS('',3,(#12188,#12189,#12190,#12191,#12192,
#12193,#12194,#12195,#12196,#12197),.UNSPECIFIED.,.F.,.F.,(4,1,1,1,1,1,
1,4),(109.955742875643,110.705579838391,111.704030252291,112.70248066619,
113.70093108009,114.69938149399,115.69783190789,116.238928182822),
 .UNSPECIFIED.);
#1622=B_SPLINE_CURVE_WITH_KNOTS('',3,(#12198,#12199,#12200,#12201,#12202,
#12203,#12204,#12205,#12206,#12207),.UNSPECIFIED.,.F.,.F.,(4,1,1,1,1,1,
1,4),(109.955742875643,110.249639861355,111.248090275255,112.246540689155,
113.244991103055,114.243441516955,115.241891930855,116.238928182822),
 .UNSPECIFIED.);
#1623=B_SPLINE_CURVE_WITH_KNOTS('',3,(#12212,#12213,#12214,#12215,#12216,
#12217,#12218,#12219,#12220,#12221,#12222),.UNSPECIFIED.,.F.,.F.,(4,1,1,
1,1,1,1,1,4),(103.672557568463,103.716426941092,104.714877354992,105.713327768892,
106.711778182792,107.710228596691,108.708679010591,109.707129424491,109.955742875643),
 .UNSPECIFIED.);
#1624=B_SPLINE_CURVE_WITH_KNOTS('',3,(#12223,#12224,#12225,#12226,#12227,
#12228,#12229,#12230,#12231,#12232),.UNSPECIFIED.,.F.,.F.,(4,1,1,1,1,1,
1,4),(103.672557568463,104.258937377956,105.257387791856,106.255838205756,
107.254288619656,108.252739033556,109.251189447456,109.955742875643),
 .UNSPECIFIED.);
#1625=B_SPLINE_CURVE_WITH_KNOTS('',3,(#12237,#12238,#12239,#12240,#12241,
#12242,#12243,#12244,#12245,#12246),.UNSPECIFIED.,.F.,.F.,(4,1,1,1,1,1,
1,4),(97.3893722612835,97.725724457693,98.7241748715929,99.7226252854927,
100.721075699393,101.719526113292,102.717976527192,103.672557568463),
 .UNSPECIFIED.);
#1626=B_SPLINE_CURVE_WITH_KNOTS('',3,(#12247,#12248,#12249,#12250,#12251,
#12252,#12253,#12254,#12255,#12256),.UNSPECIFIED.,.F.,.F.,(4,1,1,1,1,1,
1,4),(97.3893722612835,98.2682348945574,99.2666853084573,100.265135722357,
101.263586136257,102.262036550157,103.260486964057,103.672557568463),
 .UNSPECIFIED.);
#1627=B_SPLINE_CURVE_WITH_KNOTS('',3,(#12261,#12262,#12263,#12264,#12265,
#12266,#12267,#12268,#12269,#12270),.UNSPECIFIED.,.F.,.F.,(4,1,1,1,1,1,
1,4),(91.106186954104,91.7350219742941,92.7334723881939,93.7319228020937,
94.7303732159936,95.7288236298934,96.7272740437932,97.3893722612835),
 .UNSPECIFIED.);
#1628=B_SPLINE_CURVE_WITH_KNOTS('',3,(#12271,#12272,#12273,#12274,#12275,
#12276,#12277,#12278,#12279,#12280,#12281),.UNSPECIFIED.,.F.,.F.,(4,1,1,
1,1,1,1,1,4),(91.106186954104,91.2790819972586,92.2775324111584,93.2759828250583,
94.2744332389581,95.2728836528579,96.2713340667578,97.2697844806576,97.3893722612835),
 .UNSPECIFIED.);
#1629=B_SPLINE_CURVE_WITH_KNOTS('',3,(#12286,#12287,#12288,#12289,#12290,
#12291,#12292,#12293,#12294,#12295),.UNSPECIFIED.,.F.,.F.,(4,1,1,1,1,1,
1,4),(84.8230016469244,85.7443194908951,86.7427699047949,87.7412203186948,
88.7396707325946,89.7381211464944,90.7365715603942,91.106186954104),
 .UNSPECIFIED.);
#1630=B_SPLINE_CURVE_WITH_KNOTS('',3,(#12296,#12297,#12298,#12299,#12300,
#12301,#12302,#12303,#12304,#12305),.UNSPECIFIED.,.F.,.F.,(4,1,1,1,1,1,
1,4),(84.8230016469244,85.2883795138596,86.2868299277595,87.2852803416593,
88.2837307555591,89.282181169459,90.2806315833588,91.106186954104),
 .UNSPECIFIED.);
#1631=B_SPLINE_CURVE_WITH_KNOTS('',3,(#12310,#12311,#12312,#12313,#12314,
#12315,#12316,#12317,#12318,#12319,#12320),.UNSPECIFIED.,.F.,.F.,(4,1,1,
1,1,1,1,1,4),(78.5398163397448,78.7551665935963,79.7536170074961,80.7520674213959,
81.7505178352958,82.7489682491956,83.7474186630954,84.7458690769953,84.8230016469244),
 .UNSPECIFIED.);
#1632=B_SPLINE_CURVE_WITH_KNOTS('',3,(#12321,#12322,#12323,#12324,#12325,
#12326,#12327,#12328,#12329,#12330),.UNSPECIFIED.,.F.,.F.,(4,1,1,1,1,1,
1,4),(78.5398163397448,79.2976770304607,80.2961274443605,81.2945778582603,
82.2930282721602,83.29147868606,84.2899290999598,84.8230016469244),
 .UNSPECIFIED.);
#1633=B_SPLINE_CURVE_WITH_KNOTS('',3,(#12335,#12336,#12337,#12338,#12339,
#12340,#12341,#12342,#12343,#12344),.UNSPECIFIED.,.F.,.F.,(4,1,1,1,1,1,
1,4),(72.2566310325652,72.7644641101973,73.7629145240972,74.761364937997,
75.7598153518968,76.7582657657966,77.7567161796965,78.5398163397448),
 .UNSPECIFIED.);
#1634=B_SPLINE_CURVE_WITH_KNOTS('',3,(#12345,#12346,#12347,#12348,#12349,
#12350,#12351,#12352,#12353,#12354,#12355),.UNSPECIFIED.,.F.,.F.,(4,1,1,
1,1,1,1,1,4),(72.2566310325652,72.3085241331619,73.3069745470617,74.3054249609615,
75.3038753748613,76.3023257887612,77.300776202661,78.2992266165608,78.5398163397448),
 .UNSPECIFIED.);
#1635=B_SPLINE_CURVE_WITH_KNOTS('',3,(#12360,#12361,#12362,#12363,#12364,
#12365,#12366,#12367,#12368,#12369),.UNSPECIFIED.,.F.,.F.,(4,1,1,1,1,1,
1,4),(65.9734457253856,66.7737616267983,67.7722120406982,68.770662454598,
69.7691128684978,70.7675632823977,71.7660136962975,72.2566310325652),
 .UNSPECIFIED.);
#1636=B_SPLINE_CURVE_WITH_KNOTS('',3,(#12370,#12371,#12372,#12373,#12374,
#12375,#12376,#12377,#12378,#12379),.UNSPECIFIED.,.F.,.F.,(4,1,1,1,1,1,
1,4),(65.9734457253856,66.3178216497629,67.3162720636627,68.3147224775625,
69.3131728914624,70.3116233053622,71.310073719262,72.2566310325652),
 .UNSPECIFIED.);
#1637=B_SPLINE_CURVE_WITH_KNOTS('',3,(#12384,#12385,#12386,#12387,#12388,
#12389,#12390,#12391,#12392,#12393,#12394),.UNSPECIFIED.,.F.,.F.,(4,1,1,
1,1,1,1,1,4),(59.690260418206,59.7846087294995,60.7830591433994,61.7815095572992,
62.779959971199,63.7784103850989,64.7768607989987,65.7753112128985,65.9734457253856),
 .UNSPECIFIED.);
#1638=B_SPLINE_CURVE_WITH_KNOTS('',3,(#12395,#12396,#12397,#12398,#12399,
#12400,#12401,#12402,#12403,#12404),.UNSPECIFIED.,.F.,.F.,(4,1,1,1,1,1,
1,4),(59.690260418206,60.3271191663639,61.3255695802637,62.3240199941636,
63.3224704080634,64.3209208219632,65.3193712358631,65.9734457253856),
 .UNSPECIFIED.);
#1639=B_SPLINE_CURVE_WITH_KNOTS('',3,(#12409,#12410,#12411,#12412,#12413,
#12414,#12415,#12416,#12417,#12418),.UNSPECIFIED.,.F.,.F.,(4,1,1,1,1,1,
1,4),(53.4070751110264,53.7939062461006,54.7923566600004,55.7908070739002,
56.7892574878001,57.7877079016999,58.7861583155997,59.690260418206),
 .UNSPECIFIED.);
#1640=B_SPLINE_CURVE_WITH_KNOTS('',3,(#12419,#12420,#12421,#12422,#12423,
#12424,#12425,#12426,#12427,#12428),.UNSPECIFIED.,.F.,.F.,(4,1,1,1,1,1,
1,4),(53.4070751110264,54.3364166829649,55.3348670968648,56.3333175107646,
57.3317679246644,58.3302183385643,59.3286687524641,59.690260418206),
 .UNSPECIFIED.);
#1641=B_SPLINE_CURVE_WITH_KNOTS('',3,(#12433,#12434,#12435,#12436,#12437,
#12438,#12439,#12440,#12441,#12442),.UNSPECIFIED.,.F.,.F.,(4,1,1,1,1,1,
1,4),(47.1238898038468,47.8032037627016,48.8016541766014,49.8001045905012,
50.7985550044011,51.7970054183009,52.7954558322007,53.4070751110264),
 .UNSPECIFIED.);
#1642=B_SPLINE_CURVE_WITH_KNOTS('',3,(#12443,#12444,#12445,#12446,#12447,
#12448,#12449,#12450,#12451,#12452,#12453),.UNSPECIFIED.,.F.,.F.,(4,1,1,
1,1,1,1,1,4),(47.1238898038468,47.3472637856661,48.345714199566,49.3441646134658,
50.3426150273656,51.3410654412654,52.3395158551653,53.3379662690651,53.4070751110264),
 .UNSPECIFIED.);
#1643=B_SPLINE_CURVE_WITH_KNOTS('',3,(#12458,#12459,#12460,#12461,#12462,
#12463,#12464,#12465,#12466,#12467),.UNSPECIFIED.,.F.,.F.,(4,1,1,1,1,1,
1,4),(40.8407044966672,41.8125012793026,42.8109516932024,43.8094021071023,
44.8078525210021,45.8063029349019,46.8047533488018,47.1238898038468),
 .UNSPECIFIED.);
#1644=B_SPLINE_CURVE_WITH_KNOTS('',3,(#12468,#12469,#12470,#12471,#12472,
#12473,#12474,#12475,#12476,#12477),.UNSPECIFIED.,.F.,.F.,(4,1,1,1,1,1,
1,4),(40.8407044966672,41.3565613022671,42.355011716167,43.3534621300668,
44.3519125439666,45.3503629578665,46.3488133717663,47.1238898038468),
 .UNSPECIFIED.);
#1645=B_SPLINE_CURVE_WITH_KNOTS('',3,(#12482,#12483,#12484,#12485,#12486,
#12487,#12488,#12489,#12490,#12491,#12492),.UNSPECIFIED.,.F.,.F.,(4,1,1,
1,1,1,1,1,4),(34.5575191894876,34.8233483820038,35.8217987959036,36.8202492098035,
37.8186996237033,38.8171500376031,39.815600451503,40.8140508654028,40.8407044966672),
 .UNSPECIFIED.);
#1646=B_SPLINE_CURVE_WITH_KNOTS('',3,(#12493,#12494,#12495,#12496,#12497,
#12498,#12499,#12500,#12501,#12502),.UNSPECIFIED.,.F.,.F.,(4,1,1,1,1,1,
1,4),(34.5575191894876,35.3658588188682,36.364309232768,37.3627596466678,
38.3612100605677,39.3596604744675,40.3581108883673,40.8407044966672),
 .UNSPECIFIED.);
#1647=B_SPLINE_CURVE_WITH_KNOTS('',3,(#12507,#12508,#12509,#12510,#12511,
#12512,#12513,#12514,#12515,#12516),.UNSPECIFIED.,.F.,.F.,(4,1,1,1,1,1,
1,4),(28.274333882308,28.8326458986048,29.8310963125047,30.8295467264045,
31.8279971403043,32.8264475542042,33.824897968104,34.5575191894876),
 .UNSPECIFIED.);
#1648=B_SPLINE_CURVE_WITH_KNOTS('',3,(#12517,#12518,#12519,#12520,#12521,
#12522,#12523,#12524,#12525,#12526,#12527),.UNSPECIFIED.,.F.,.F.,(4,1,1,
1,1,1,1,1,4),(28.274333882308,28.3767059215694,29.3751563354692,30.373606749369,
31.3720571632689,32.3705075771687,33.3689579910685,34.3674084049683,34.5575191894876),
 .UNSPECIFIED.);
#1649=B_SPLINE_CURVE_WITH_KNOTS('',3,(#12532,#12533,#12534,#12535,#12536,
#12537,#12538,#12539,#12540,#12541),.UNSPECIFIED.,.F.,.F.,(4,1,1,1,1,1,
1,4),(21.9911485751285,22.8419434152059,23.8403938291057,24.8388442430055,
25.8372946569053,26.8357450708052,27.834195484705,28.274333882308),
 .UNSPECIFIED.);
#1650=B_SPLINE_CURVE_WITH_KNOTS('',3,(#12542,#12543,#12544,#12545,#12546,
#12547,#12548,#12549,#12550,#12551),.UNSPECIFIED.,.F.,.F.,(4,1,1,1,1,1,
1,4),(21.9911485751285,22.3860034381704,23.3844538520702,24.38290426597,
25.3813546798699,26.3798050937697,27.3782555076695,28.274333882308),
 .UNSPECIFIED.);
#1651=B_SPLINE_CURVE_WITH_KNOTS('',3,(#12557,#12558,#12559,#12560,#12561),
 .UNSPECIFIED.,.F.,.F.,(4,1,4),(14.3984001269718,15.3968505408716,15.7079632679489),
 .UNSPECIFIED.);
#1652=B_SPLINE_CURVE_WITH_KNOTS('',3,(#12564,#12565,#12566,#12567,#12568),
 .UNSPECIFIED.,.F.,.F.,(4,1,4),(13.8759337553362,14.8543401040072,15.7079632679489),
 .UNSPECIFIED.);
#1653=B_SPLINE_CURVE_WITH_KNOTS('',3,(#12574,#12575,#12576,#12577),
 .UNSPECIFIED.,.F.,.F.,(4,4),(108.12371336303,108.831095115081),
 .UNSPECIFIED.);
#1654=B_SPLINE_CURVE_WITH_KNOTS('',3,(#12585,#12586,#12587,#12588,#12589,
#12590,#12591,#12592,#12593,#12594),.UNSPECIFIED.,.F.,.F.,(4,3,3,4),(-106.814150222053,
-105.835743873382,-104.837293459482,-104.379939320515),.UNSPECIFIED.);
#1655=B_SPLINE_CURVE_WITH_KNOTS('',3,(#12599,#12600,#12601,#12602,#12603,
#12604,#12605,#12606,#12607,#12608,#12609,#12610,#12611,#12612,#12613,#12614,
#12615,#12616,#12617,#12618,#12619,#12620),.UNSPECIFIED.,.F.,.F.,(4,3,3,
3,3,3,3,4),(101.84052805585,102.840392631682,103.838843045582,104.837293459482,
105.835743873382,106.834194287282,107.832644701182,108.12371336303),
 .UNSPECIFIED.);
#1656=B_SPLINE_CURVE_WITH_KNOTS('',3,(#12621,#12622,#12623,#12624,#12625,
#12626,#12627,#12628,#12629,#12630,#12631,#12632,#12633,#12634,#12635,#12636,
#12637,#12638,#12639,#12640,#12641,#12642),.UNSPECIFIED.,.F.,.F.,(4,3,3,
3,3,3,3,4),(-104.379939320515,-103.838843045582,-102.840392631682,-101.841942217783,
-100.843491803883,-99.8450413899829,-98.8465909760831,-98.096754013335),
 .UNSPECIFIED.);
#1657=B_SPLINE_CURVE_WITH_KNOTS('',3,(#12647,#12648,#12649,#12650,#12651,
#12652,#12653,#12654,#12655,#12656,#12657,#12658,#12659,#12660,#12661,#12662,
#12663,#12664,#12665,#12666,#12667,#12668),.UNSPECIFIED.,.F.,.F.,(4,3,3,
3,3,3,3,4),(95.5573427486709,95.8512397343836,96.8496901482835,97.8481405621833,
98.8465909760831,99.845041389983,100.843491803883,101.84052805585),
 .UNSPECIFIED.);
#1658=B_SPLINE_CURVE_WITH_KNOTS('',3,(#12669,#12670,#12671,#12672,#12673,
#12674,#12675,#12676,#12677,#12678,#12679,#12680,#12681,#12682,#12683,#12684,
#12685,#12686,#12687,#12688,#12689,#12690,#12691,#12692,#12693),
 .UNSPECIFIED.,.F.,.F.,(4,3,3,3,3,3,3,3,4),(-98.096754013335,-97.8481405621833,
-96.8496901482835,-95.8512397343836,-94.8527893204838,-93.854338906584,
-92.8558884926841,-91.8574380787843,-91.8135687061554),.UNSPECIFIED.);
#1659=B_SPLINE_CURVE_WITH_KNOTS('',3,(#12698,#12699,#12700,#12701,#12702,
#12703,#12704,#12705,#12706,#12707,#12708,#12709,#12710,#12711,#12712,#12713,
#12714,#12715,#12716,#12717,#12718,#12719),.UNSPECIFIED.,.F.,.F.,(4,3,3,
3,3,3,3,4),(89.2741574414913,89.8605372509847,90.8589876648845,91.8574380787843,
92.8558884926841,93.854338906584,94.8527893204838,95.5573427486709),
 .UNSPECIFIED.);
#1660=B_SPLINE_CURVE_WITH_KNOTS('',3,(#12720,#12721,#12722,#12723,#12724,
#12725,#12726,#12727,#12728,#12729,#12730,#12731,#12732,#12733,#12734,#12735,
#12736,#12737,#12738,#12739,#12740,#12741),.UNSPECIFIED.,.F.,.F.,(4,3,3,
3,3,3,3,4),(-91.8135687061554,-90.8589876648845,-89.8605372509847,-88.8620868370848,
-87.863636423185,-86.8651860092852,-85.8667355953854,-85.5303833989758),
 .UNSPECIFIED.);
#1661=B_SPLINE_CURVE_WITH_KNOTS('',3,(#12746,#12747,#12748,#12749,#12750,
#12751,#12752,#12753,#12754,#12755,#12756,#12757,#12758,#12759,#12760,#12761,
#12762,#12763,#12764,#12765,#12766,#12767),.UNSPECIFIED.,.F.,.F.,(4,3,3,
3,3,3,3,4),(82.9909721343117,83.8698347675857,84.8682851814855,85.8667355953853,
86.8651860092852,87.863636423185,88.8620868370848,89.2741574414913),
 .UNSPECIFIED.);
#1662=B_SPLINE_CURVE_WITH_KNOTS('',3,(#12768,#12769,#12770,#12771,#12772,
#12773,#12774,#12775,#12776,#12777,#12778,#12779,#12780,#12781,#12782,#12783,
#12784,#12785,#12786,#12787,#12788,#12789),.UNSPECIFIED.,.F.,.F.,(4,3,3,
3,3,3,3,4),(-85.5303833989758,-84.8682851814855,-83.8698347675857,-82.8713843536858,
-81.872933939786,-80.8744835258862,-79.8760331119864,-79.2471980917962),
 .UNSPECIFIED.);
#1663=B_SPLINE_CURVE_WITH_KNOTS('',3,(#12794,#12795,#12796,#12797,#12798,
#12799,#12800,#12801,#12802,#12803,#12804,#12805,#12806,#12807,#12808,#12809,
#12810,#12811,#12812,#12813,#12814,#12815,#12816,#12817,#12818),
 .UNSPECIFIED.,.F.,.F.,(4,3,3,3,3,3,3,3,4),(76.7077868271321,76.8806818702869,
77.8791322841867,78.8775826980865,79.8760331119864,80.8744835258862,81.872933939786,
82.8713843536859,82.9909721343117),.UNSPECIFIED.);
#1664=B_SPLINE_CURVE_WITH_KNOTS('',3,(#12819,#12820,#12821,#12822,#12823,
#12824,#12825,#12826,#12827,#12828,#12829,#12830,#12831,#12832,#12833,#12834,
#12835,#12836,#12837,#12838,#12839,#12840),.UNSPECIFIED.,.F.,.F.,(4,3,3,
3,3,3,3,4),(-79.2471980917962,-78.8775826980865,-77.8791322841867,-76.8806818702869,
-75.882231456387,-74.8837810424872,-73.8853306285874,-72.9640127846166),
 .UNSPECIFIED.);
#1665=B_SPLINE_CURVE_WITH_KNOTS('',3,(#12845,#12846,#12847,#12848,#12849,
#12850,#12851,#12852,#12853,#12854,#12855,#12856,#12857,#12858,#12859,#12860,
#12861,#12862,#12863,#12864,#12865,#12866),.UNSPECIFIED.,.F.,.F.,(4,3,3,
3,3,3,3,4),(70.4246015199525,70.8899793868879,71.8884298007877,72.8868802146876,
73.8853306285874,74.8837810424872,75.882231456387,76.7077868271321),
 .UNSPECIFIED.);
#1666=B_SPLINE_CURVE_WITH_KNOTS('',3,(#12867,#12868,#12869,#12870,#12871,
#12872,#12873,#12874,#12875,#12876,#12877,#12878,#12879,#12880,#12881,#12882,
#12883,#12884,#12885,#12886,#12887,#12888,#12889,#12890,#12891),
 .UNSPECIFIED.,.F.,.F.,(4,3,3,3,3,3,3,3,4),(-72.9640127846166,-72.8868802146875,
-71.8884298007877,-70.8899793868879,-69.8915289729881,-68.8930785590882,
-67.8946281451884,-66.8961777312886,-66.680827477437),.UNSPECIFIED.);
#1667=B_SPLINE_CURVE_WITH_KNOTS('',3,(#12896,#12897,#12898,#12899,#12900,
#12901,#12902,#12903,#12904,#12905,#12906,#12907,#12908,#12909,#12910,#12911,
#12912,#12913,#12914,#12915,#12916,#12917),.UNSPECIFIED.,.F.,.F.,(4,3,3,
3,3,3,3,4),(64.1414162127729,64.8992769034889,65.8977273173887,66.8961777312886,
67.8946281451884,68.8930785590882,69.8915289729881,70.4246015199525),
 .UNSPECIFIED.);
#1668=B_SPLINE_CURVE_WITH_KNOTS('',3,(#12918,#12919,#12920,#12921,#12922,
#12923,#12924,#12925,#12926,#12927,#12928,#12929,#12930,#12931,#12932,#12933,
#12934,#12935,#12936,#12937,#12938,#12939),.UNSPECIFIED.,.F.,.F.,(4,3,3,
3,3,3,3,4),(-66.680827477437,-65.8977273173887,-64.8992769034889,-63.9008264895891,
-62.9023760756892,-61.9039256617894,-60.9054752478896,-60.3976421702574),
 .UNSPECIFIED.);
#1669=B_SPLINE_CURVE_WITH_KNOTS('',3,(#12944,#12945,#12946,#12947,#12948,
#12949,#12950,#12951,#12952,#12953,#12954,#12955,#12956,#12957,#12958,#12959,
#12960,#12961,#12962,#12963,#12964,#12965,#12966,#12967,#12968),
 .UNSPECIFIED.,.F.,.F.,(4,3,3,3,3,3,3,3,4),(57.8582309055933,57.9101240061901,
58.9085744200899,59.9070248339898,60.9054752478896,61.9039256617894,62.9023760756893,
63.9008264895891,64.1414162127729),.UNSPECIFIED.);
#1670=B_SPLINE_CURVE_WITH_KNOTS('',3,(#12969,#12970,#12971,#12972,#12973,
#12974,#12975,#12976,#12977,#12978,#12979,#12980,#12981,#12982,#12983,#12984,
#12985,#12986,#12987,#12988,#12989,#12990),.UNSPECIFIED.,.F.,.F.,(4,3,3,
3,3,3,3,4),(-60.3976421702574,-59.9070248339898,-58.9085744200899,-57.9101240061901,
-56.9116735922903,-55.9132231783904,-54.9147727644906,-54.1144568630778),
 .UNSPECIFIED.);
#1671=B_SPLINE_CURVE_WITH_KNOTS('',3,(#12995,#12996,#12997,#12998,#12999,
#13000,#13001,#13002,#13003,#13004,#13005,#13006,#13007,#13008,#13009,#13010,
#13011,#13012,#13013,#13014,#13015,#13016),.UNSPECIFIED.,.F.,.F.,(4,3,3,
3,3,3,3,4),(51.5750455984138,51.9194215227911,52.917871936691,53.9163223505908,
54.9147727644906,55.9132231783905,56.9116735922903,57.8582309055933),
 .UNSPECIFIED.);
#1672=B_SPLINE_CURVE_WITH_KNOTS('',3,(#13017,#13018,#13019,#13020,#13021,
#13022,#13023,#13024,#13025,#13026,#13027,#13028,#13029,#13030,#13031,#13032,
#13033,#13034,#13035,#13036,#13037,#13038,#13039,#13040,#13041),
 .UNSPECIFIED.,.F.,.F.,(4,3,3,3,3,3,3,3,4),(-54.1144568630778,-53.9163223505908,
-52.917871936691,-51.9194215227911,-50.9209711088913,-49.9225206949915,
-48.9240702810916,-47.9256198671918,-47.8312715558982),.UNSPECIFIED.);
#1673=B_SPLINE_CURVE_WITH_KNOTS('',3,(#13046,#13047,#13048,#13049,#13050,
#13051,#13052,#13053,#13054,#13055,#13056,#13057,#13058,#13059,#13060,#13061,
#13062,#13063,#13064,#13065,#13066,#13067),.UNSPECIFIED.,.F.,.F.,(4,3,3,
3,3,3,3,4),(45.2918602912342,45.9287190393922,46.927169453292,47.9256198671918,
48.9240702810917,49.9225206949915,50.9209711088913,51.5750455984138),
 .UNSPECIFIED.);
#1674=B_SPLINE_CURVE_WITH_KNOTS('',3,(#13068,#13069,#13070,#13071,#13072,
#13073,#13074,#13075,#13076,#13077,#13078,#13079,#13080,#13081,#13082,#13083,
#13084,#13085,#13086,#13087,#13088,#13089),.UNSPECIFIED.,.F.,.F.,(4,3,3,
3,3,3,3,4),(-47.8312715558982,-46.927169453292,-45.9287190393921,-44.9302686254923,
-43.9318182115925,-42.9333677976927,-41.9349173837928,-41.5480862487186),
 .UNSPECIFIED.);
#1675=B_SPLINE_CURVE_WITH_KNOTS('',3,(#13094,#13095,#13096,#13097,#13098,
#13099,#13100,#13101,#13102,#13103,#13104,#13105,#13106,#13107,#13108,#13109,
#13110,#13111,#13112,#13113,#13114,#13115),.UNSPECIFIED.,.F.,.F.,(4,3,3,
3,3,3,3,4),(39.0086749840546,39.9380165559932,40.936466969893,41.9349173837928,
42.9333677976927,43.9318182115925,44.9302686254923,45.2918602912342),
 .UNSPECIFIED.);
#1676=B_SPLINE_CURVE_WITH_KNOTS('',3,(#13116,#13117,#13118,#13119,#13120,
#13121,#13122,#13123,#13124,#13125,#13126,#13127,#13128,#13129,#13130,#13131,
#13132,#13133,#13134,#13135,#13136,#13137),.UNSPECIFIED.,.F.,.F.,(4,3,3,
3,3,3,3,4),(-41.5480862487186,-40.936466969893,-39.9380165559932,-38.9395661420933,
-37.9411157281935,-36.9426653142937,-35.9442149003939,-35.2649009415391),
 .UNSPECIFIED.);
#1677=B_SPLINE_CURVE_WITH_KNOTS('',3,(#13142,#13143,#13144,#13145,#13146,
#13147,#13148,#13149,#13150,#13151,#13152,#13153,#13154,#13155,#13156,#13157,
#13158,#13159,#13160,#13161,#13162,#13163,#13164,#13165,#13166),
 .UNSPECIFIED.,.F.,.F.,(4,3,3,3,3,3,3,3,4),(32.725489676875,32.9488636586944,
33.9473140725942,34.945764486494,35.9442149003939,36.9426653142937,37.9411157281935,
38.9395661420934,39.0086749840546),.UNSPECIFIED.);
#1678=B_SPLINE_CURVE_WITH_KNOTS('',3,(#13167,#13168,#13169,#13170,#13171,
#13172,#13173,#13174,#13175,#13176,#13177,#13178,#13179,#13180,#13181,#13182,
#13183,#13184,#13185,#13186,#13187,#13188),.UNSPECIFIED.,.F.,.F.,(4,3,3,
3,3,3,3,4),(-35.2649009415391,-34.945764486494,-33.9473140725942,-32.9488636586944,
-31.9504132447945,-30.9519628308947,-29.9535124169949,-28.9817156343595),
 .UNSPECIFIED.);
#1679=B_SPLINE_CURVE_WITH_KNOTS('',3,(#13193,#13194,#13195,#13196,#13197,
#13198,#13199,#13200,#13201,#13202,#13203,#13204,#13205,#13206,#13207,#13208,
#13209,#13210,#13211,#13212,#13213,#13214),.UNSPECIFIED.,.F.,.F.,(4,3,3,
3,3,3,3,4),(26.4423043696954,26.9581611752954,27.9566115891952,28.9550620030951,
29.9535124169949,30.9519628308947,31.9504132447945,32.725489676875),
 .UNSPECIFIED.);
#1680=B_SPLINE_CURVE_WITH_KNOTS('',3,(#13215,#13216,#13217,#13218,#13219,
#13220,#13221,#13222,#13223,#13224,#13225,#13226,#13227,#13228,#13229,#13230,
#13231,#13232,#13233,#13234,#13235,#13236,#13237,#13238,#13239),
 .UNSPECIFIED.,.F.,.F.,(4,3,3,3,3,3,3,3,4),(-28.9817156343595,-28.955062003095,
-27.9566115891952,-26.9581611752954,-25.9597107613956,-24.9612603474957,
-23.9628099335959,-22.9643595196961,-22.6985303271799),.UNSPECIFIED.);
#1681=B_SPLINE_CURVE_WITH_KNOTS('',3,(#13244,#13245,#13246,#13247,#13248,
#13249,#13250,#13251,#13252,#13253,#13254,#13255,#13256,#13257,#13258,#13259,
#13260,#13261,#13262,#13263,#13264,#13265),.UNSPECIFIED.,.F.,.F.,(4,3,3,
3,3,3,3,4),(20.1591190625158,20.9674586918964,21.9659091057963,22.9643595196961,
23.9628099335959,24.9612603474957,25.9597107613956,26.4423043696954),
 .UNSPECIFIED.);
#1682=B_SPLINE_CURVE_WITH_KNOTS('',3,(#13266,#13267,#13268,#13269,#13270,
#13271,#13272,#13273,#13274,#13275,#13276,#13277,#13278,#13279,#13280,#13281,
#13282,#13283,#13284,#13285,#13286,#13287),.UNSPECIFIED.,.F.,.F.,(4,3,3,
3,3,3,3,4),(-22.6985303271799,-21.9659091057962,-20.9674586918964,-19.9690082779966,
-18.9705578640968,-17.9721074501969,-16.9736570362971,-16.4153450200003),
 .UNSPECIFIED.);
#1683=B_SPLINE_CURVE_WITH_KNOTS('',3,(#13292,#13293,#13294,#13295,#13296,
#13297,#13298,#13299,#13300,#13301,#13302,#13303,#13304,#13305,#13306,#13307,
#13308,#13309,#13310,#13311,#13312,#13313,#13314,#13315,#13316),
 .UNSPECIFIED.,.F.,.F.,(4,3,3,3,3,3,3,3,4),(13.8759337553362,13.9783057945976,
14.9767562084975,15.9752066223973,16.9736570362971,17.9721074501969,18.9705578640968,
19.9690082779966,20.1591190625158),.UNSPECIFIED.);
#1684=B_SPLINE_CURVE_WITH_KNOTS('',3,(#13317,#13318,#13319,#13320,#13321,
#13322,#13323,#13324,#13325,#13326,#13327,#13328,#13329,#13330,#13331,#13332,
#13333,#13334,#13335,#13336,#13337,#13338),.UNSPECIFIED.,.F.,.F.,(4,3,3,
3,3,3,3,4),(-16.4153450200003,-15.9752066223973,-14.9767562084974,-13.9783057945976,
-12.9798553806978,-11.9814049667979,-10.9829545528981,-10.1321597128207),
 .UNSPECIFIED.);
#1685=B_SPLINE_CURVE_WITH_KNOTS('',3,(#13344,#13345,#13346,#13347,#13348,
#13349,#13350,#13351,#13352,#13353,#13354,#13355,#13356),.UNSPECIFIED.,
 .F.,.F.,(4,3,3,3,4),(-3.84897440564112,-2.99535124169948,-1.99690082779965,
-0.998450413899823,0.),.UNSPECIFIED.);
#1686=B_SPLINE_CURVE_WITH_KNOTS('',3,(#13359,#13360,#13361,#13362,#13363,
#13364,#13365,#13366,#13367,#13368,#13369,#13370,#13371,#13372,#13373,#13374,
#13375,#13376,#13377),.UNSPECIFIED.,.F.,.F.,(4,3,3,3,3,3,4),(2.01694489302834,
2.99535124169949,3.99380165559932,4.99225206949915,5.99070248339898,6.98915289729881,
7.59274844815663),.UNSPECIFIED.);
#1687=B_SPLINE_CURVE_WITH_KNOTS('',3,(#13383,#13384,#13385,#13386,#13387,
#13388,#13389,#13390),.UNSPECIFIED.,.F.,.F.,(4,1,1,1,1,4),(116.238928182822,
116.69628232179,117.69473273569,118.693183149589,119.691633563489,120.690083977389),
 .UNSPECIFIED.);
#1688=B_SPLINE_CURVE_WITH_KNOTS('',3,(#13393,#13394,#13395,#13396,#13397,
#13398,#13399,#13400,#13401),.UNSPECIFIED.,.F.,.F.,(4,1,1,1,1,1,4),(116.238928182822,
116.240342344754,117.238792758654,118.237243172554,119.235693586454,120.234144000354,
121.212550349025),.UNSPECIFIED.);
#1689=B_SPLINE_CURVE_WITH_KNOTS('',3,(#13406,#13407,#13408,#13409,#13410,
#13411,#13412,#13413,#13414,#13415),.UNSPECIFIED.,.F.,.F.,(4,1,1,1,1,1,
1,4),(109.955742875643,110.705579838391,111.704030252291,112.70248066619,
113.70093108009,114.69938149399,115.69783190789,116.238928182822),
 .UNSPECIFIED.);
#1690=B_SPLINE_CURVE_WITH_KNOTS('',3,(#13416,#13417,#13418,#13419,#13420,
#13421,#13422,#13423,#13424,#13425),.UNSPECIFIED.,.F.,.F.,(4,1,1,1,1,1,
1,4),(109.955742875643,110.249639861355,111.248090275255,112.246540689155,
113.244991103055,114.243441516955,115.241891930855,116.238928182822),
 .UNSPECIFIED.);
#1691=B_SPLINE_CURVE_WITH_KNOTS('',3,(#13430,#13431,#13432,#13433,#13434,
#13435,#13436,#13437,#13438,#13439,#13440),.UNSPECIFIED.,.F.,.F.,(4,1,1,
1,1,1,1,1,4),(103.672557568463,103.716426941092,104.714877354992,105.713327768892,
106.711778182792,107.710228596691,108.708679010591,109.707129424491,109.955742875643),
 .UNSPECIFIED.);
#1692=B_SPLINE_CURVE_WITH_KNOTS('',3,(#13441,#13442,#13443,#13444,#13445,
#13446,#13447,#13448,#13449,#13450),.UNSPECIFIED.,.F.,.F.,(4,1,1,1,1,1,
1,4),(103.672557568463,104.258937377956,105.257387791856,106.255838205756,
107.254288619656,108.252739033556,109.251189447456,109.955742875643),
 .UNSPECIFIED.);
#1693=B_SPLINE_CURVE_WITH_KNOTS('',3,(#13455,#13456,#13457,#13458,#13459,
#13460,#13461,#13462,#13463,#13464),.UNSPECIFIED.,.F.,.F.,(4,1,1,1,1,1,
1,4),(97.3893722612836,97.7257244576931,98.7241748715929,99.7226252854927,
100.721075699393,101.719526113292,102.717976527192,103.672557568463),
 .UNSPECIFIED.);
#1694=B_SPLINE_CURVE_WITH_KNOTS('',3,(#13465,#13466,#13467,#13468,#13469,
#13470,#13471,#13472,#13473,#13474),.UNSPECIFIED.,.F.,.F.,(4,1,1,1,1,1,
1,4),(97.3893722612835,98.2682348945574,99.2666853084572,100.265135722357,
101.263586136257,102.262036550157,103.260486964057,103.672557568463),
 .UNSPECIFIED.);
#1695=B_SPLINE_CURVE_WITH_KNOTS('',3,(#13479,#13480,#13481,#13482,#13483,
#13484,#13485,#13486,#13487,#13488),.UNSPECIFIED.,.F.,.F.,(4,1,1,1,1,1,
1,4),(91.106186954104,91.7350219742941,92.7334723881939,93.7319228020937,
94.7303732159936,95.7288236298934,96.7272740437932,97.3893722612836),
 .UNSPECIFIED.);
#1696=B_SPLINE_CURVE_WITH_KNOTS('',3,(#13489,#13490,#13491,#13492,#13493,
#13494,#13495,#13496,#13497,#13498,#13499),.UNSPECIFIED.,.F.,.F.,(4,1,1,
1,1,1,1,1,4),(91.106186954104,91.2790819972586,92.2775324111584,93.2759828250583,
94.2744332389581,95.2728836528579,96.2713340667578,97.2697844806576,97.3893722612835),
 .UNSPECIFIED.);
#1697=B_SPLINE_CURVE_WITH_KNOTS('',3,(#13504,#13505,#13506,#13507,#13508,
#13509,#13510,#13511,#13512,#13513),.UNSPECIFIED.,.F.,.F.,(4,1,1,1,1,1,
1,4),(84.8230016469244,85.7443194908951,86.7427699047949,87.7412203186948,
88.7396707325946,89.7381211464944,90.7365715603943,91.106186954104),
 .UNSPECIFIED.);
#1698=B_SPLINE_CURVE_WITH_KNOTS('',3,(#13514,#13515,#13516,#13517,#13518,
#13519,#13520,#13521,#13522,#13523),.UNSPECIFIED.,.F.,.F.,(4,1,1,1,1,1,
1,4),(84.8230016469244,85.2883795138596,86.2868299277595,87.2852803416593,
88.2837307555591,89.282181169459,90.2806315833588,91.106186954104),
 .UNSPECIFIED.);
#1699=B_SPLINE_CURVE_WITH_KNOTS('',3,(#13528,#13529,#13530,#13531,#13532,
#13533,#13534,#13535,#13536,#13537,#13538),.UNSPECIFIED.,.F.,.F.,(4,1,1,
1,1,1,1,1,4),(78.5398163397448,78.7551665935963,79.7536170074961,80.752067421396,
81.7505178352958,82.7489682491956,83.7474186630954,84.7458690769953,84.8230016469244),
 .UNSPECIFIED.);
#1700=B_SPLINE_CURVE_WITH_KNOTS('',3,(#13539,#13540,#13541,#13542,#13543,
#13544,#13545,#13546,#13547,#13548),.UNSPECIFIED.,.F.,.F.,(4,1,1,1,1,1,
1,4),(78.5398163397448,79.2976770304606,80.2961274443605,81.2945778582603,
82.2930282721601,83.29147868606,84.2899290999598,84.8230016469244),
 .UNSPECIFIED.);
#1701=B_SPLINE_CURVE_WITH_KNOTS('',3,(#13553,#13554,#13555,#13556,#13557,
#13558,#13559,#13560,#13561,#13562),.UNSPECIFIED.,.F.,.F.,(4,1,1,1,1,1,
1,4),(72.2566310325652,72.7644641101973,73.7629145240972,74.761364937997,
75.7598153518968,76.7582657657966,77.7567161796965,78.5398163397448),
 .UNSPECIFIED.);
#1702=B_SPLINE_CURVE_WITH_KNOTS('',3,(#13563,#13564,#13565,#13566,#13567,
#13568,#13569,#13570,#13571,#13572,#13573),.UNSPECIFIED.,.F.,.F.,(4,1,1,
1,1,1,1,1,4),(72.2566310325652,72.3085241331619,73.3069745470617,74.3054249609615,
75.3038753748613,76.3023257887612,77.300776202661,78.2992266165608,78.5398163397448),
 .UNSPECIFIED.);
#1703=B_SPLINE_CURVE_WITH_KNOTS('',3,(#13578,#13579,#13580,#13581,#13582,
#13583,#13584,#13585,#13586,#13587),.UNSPECIFIED.,.F.,.F.,(4,1,1,1,1,1,
1,4),(65.9734457253856,66.7737616267983,67.7722120406982,68.770662454598,
69.7691128684978,70.7675632823977,71.7660136962975,72.2566310325652),
 .UNSPECIFIED.);
#1704=B_SPLINE_CURVE_WITH_KNOTS('',3,(#13588,#13589,#13590,#13591,#13592,
#13593,#13594,#13595,#13596,#13597),.UNSPECIFIED.,.F.,.F.,(4,1,1,1,1,1,
1,4),(65.9734457253856,66.3178216497629,67.3162720636627,68.3147224775625,
69.3131728914624,70.3116233053622,71.310073719262,72.2566310325652),
 .UNSPECIFIED.);
#1705=B_SPLINE_CURVE_WITH_KNOTS('',3,(#13602,#13603,#13604,#13605,#13606,
#13607,#13608,#13609,#13610,#13611,#13612),.UNSPECIFIED.,.F.,.F.,(4,1,1,
1,1,1,1,1,4),(59.690260418206,59.7846087294995,60.7830591433994,61.7815095572992,
62.779959971199,63.7784103850989,64.7768607989987,65.7753112128985,65.9734457253856),
 .UNSPECIFIED.);
#1706=B_SPLINE_CURVE_WITH_KNOTS('',3,(#13613,#13614,#13615,#13616,#13617,
#13618,#13619,#13620,#13621,#13622),.UNSPECIFIED.,.F.,.F.,(4,1,1,1,1,1,
1,4),(59.690260418206,60.3271191663639,61.3255695802637,62.3240199941636,
63.3224704080634,64.3209208219632,65.319371235863,65.9734457253856),
 .UNSPECIFIED.);
#1707=B_SPLINE_CURVE_WITH_KNOTS('',3,(#13627,#13628,#13629,#13630,#13631,
#13632,#13633,#13634,#13635,#13636),.UNSPECIFIED.,.F.,.F.,(4,1,1,1,1,1,
1,4),(53.4070751110264,53.7939062461006,54.7923566600004,55.7908070739002,
56.7892574878,57.7877079016999,58.7861583155997,59.690260418206),
 .UNSPECIFIED.);
#1708=B_SPLINE_CURVE_WITH_KNOTS('',3,(#13637,#13638,#13639,#13640,#13641,
#13642,#13643,#13644,#13645,#13646),.UNSPECIFIED.,.F.,.F.,(4,1,1,1,1,1,
1,4),(53.4070751110264,54.3364166829649,55.3348670968648,56.3333175107646,
57.3317679246644,58.3302183385642,59.3286687524641,59.690260418206),
 .UNSPECIFIED.);
#1709=B_SPLINE_CURVE_WITH_KNOTS('',3,(#13651,#13652,#13653,#13654,#13655,
#13656,#13657,#13658,#13659,#13660),.UNSPECIFIED.,.F.,.F.,(4,1,1,1,1,1,
1,4),(47.1238898038468,47.8032037627016,48.8016541766014,49.8001045905012,
50.7985550044011,51.7970054183009,52.7954558322007,53.4070751110264),
 .UNSPECIFIED.);
#1710=B_SPLINE_CURVE_WITH_KNOTS('',3,(#13661,#13662,#13663,#13664,#13665,
#13666,#13667,#13668,#13669,#13670,#13671),.UNSPECIFIED.,.F.,.F.,(4,1,1,
1,1,1,1,1,4),(47.1238898038468,47.3472637856661,48.3457141995659,49.3441646134658,
50.3426150273656,51.3410654412654,52.3395158551653,53.3379662690651,53.4070751110264),
 .UNSPECIFIED.);
#1711=B_SPLINE_CURVE_WITH_KNOTS('',3,(#13676,#13677,#13678,#13679,#13680,
#13681,#13682,#13683,#13684,#13685),.UNSPECIFIED.,.F.,.F.,(4,1,1,1,1,1,
1,4),(40.8407044966672,41.8125012793026,42.8109516932024,43.8094021071023,
44.8078525210021,45.8063029349019,46.8047533488018,47.1238898038468),
 .UNSPECIFIED.);
#1712=B_SPLINE_CURVE_WITH_KNOTS('',3,(#13686,#13687,#13688,#13689,#13690,
#13691,#13692,#13693,#13694,#13695),.UNSPECIFIED.,.F.,.F.,(4,1,1,1,1,1,
1,4),(40.8407044966672,41.3565613022671,42.355011716167,43.3534621300668,
44.3519125439666,45.3503629578665,46.3488133717663,47.1238898038468),
 .UNSPECIFIED.);
#1713=B_SPLINE_CURVE_WITH_KNOTS('',3,(#13700,#13701,#13702,#13703,#13704,
#13705,#13706,#13707,#13708,#13709,#13710),.UNSPECIFIED.,.F.,.F.,(4,1,1,
1,1,1,1,1,4),(34.5575191894876,34.8233483820038,35.8217987959036,36.8202492098035,
37.8186996237033,38.8171500376031,39.8156004515029,40.8140508654028,40.8407044966672),
 .UNSPECIFIED.);
#1714=B_SPLINE_CURVE_WITH_KNOTS('',3,(#13711,#13712,#13713,#13714,#13715,
#13716,#13717,#13718,#13719,#13720),.UNSPECIFIED.,.F.,.F.,(4,1,1,1,1,1,
1,4),(34.5575191894876,35.3658588188682,36.364309232768,37.3627596466678,
38.3612100605677,39.3596604744675,40.3581108883673,40.8407044966672),
 .UNSPECIFIED.);
#1715=B_SPLINE_CURVE_WITH_KNOTS('',3,(#13725,#13726,#13727,#13728,#13729,
#13730,#13731,#13732,#13733,#13734),.UNSPECIFIED.,.F.,.F.,(4,1,1,1,1,1,
1,4),(28.274333882308,28.8326458986048,29.8310963125047,30.8295467264045,
31.8279971403043,32.8264475542041,33.824897968104,34.5575191894876),
 .UNSPECIFIED.);
#1716=B_SPLINE_CURVE_WITH_KNOTS('',3,(#13735,#13736,#13737,#13738,#13739,
#13740,#13741,#13742,#13743,#13744,#13745),.UNSPECIFIED.,.F.,.F.,(4,1,1,
1,1,1,1,1,4),(28.274333882308,28.3767059215694,29.3751563354692,30.373606749369,
31.3720571632688,32.3705075771687,33.3689579910685,34.3674084049683,34.5575191894876),
 .UNSPECIFIED.);
#1717=B_SPLINE_CURVE_WITH_KNOTS('',3,(#13750,#13751,#13752,#13753,#13754,
#13755,#13756,#13757,#13758,#13759),.UNSPECIFIED.,.F.,.F.,(4,1,1,1,1,1,
1,4),(21.9911485751285,22.8419434152058,23.8403938291057,24.8388442430055,
25.8372946569053,26.8357450708052,27.834195484705,28.274333882308),
 .UNSPECIFIED.);
#1718=B_SPLINE_CURVE_WITH_KNOTS('',3,(#13760,#13761,#13762,#13763,#13764,
#13765,#13766,#13767,#13768,#13769),.UNSPECIFIED.,.F.,.F.,(4,1,1,1,1,1,
1,4),(21.9911485751285,22.3860034381704,23.3844538520702,24.38290426597,
25.3813546798699,26.3798050937697,27.3782555076695,28.274333882308),
 .UNSPECIFIED.);
#1719=B_SPLINE_CURVE_WITH_KNOTS('',3,(#13775,#13776,#13777,#13778,#13779),
 .UNSPECIFIED.,.F.,.F.,(4,1,4),(14.3984001269717,15.3968505408716,15.7079632679489),
 .UNSPECIFIED.);
#1720=B_SPLINE_CURVE_WITH_KNOTS('',3,(#13782,#13783,#13784,#13785,#13786),
 .UNSPECIFIED.,.F.,.F.,(4,1,4),(13.8759337553362,14.8543401040072,15.7079632679489),
 .UNSPECIFIED.);
#1721=B_SPLINE_CURVE_WITH_KNOTS('',3,(#13792,#13793,#13794,#13795),
 .UNSPECIFIED.,.F.,.F.,(4,4),(108.12371336303,108.831095115081),
 .UNSPECIFIED.);
#1722=B_SPLINE_CURVE_WITH_KNOTS('',3,(#13803,#13804,#13805,#13806,#13807,
#13808,#13809,#13810,#13811,#13812),.UNSPECIFIED.,.F.,.F.,(4,3,3,4),(-106.814150222053,
-105.835743873382,-104.837293459482,-104.379939320515),.UNSPECIFIED.);
#1723=B_SPLINE_CURVE_WITH_KNOTS('',3,(#13817,#13818,#13819,#13820,#13821,
#13822,#13823,#13824,#13825,#13826,#13827,#13828,#13829,#13830,#13831,#13832,
#13833,#13834,#13835,#13836,#13837,#13838),.UNSPECIFIED.,.F.,.F.,(4,3,3,
3,3,3,3,4),(101.84052805585,102.840392631682,103.838843045582,104.837293459482,
105.835743873382,106.834194287282,107.832644701182,108.12371336303),
 .UNSPECIFIED.);
#1724=B_SPLINE_CURVE_WITH_KNOTS('',3,(#13839,#13840,#13841,#13842,#13843,
#13844,#13845,#13846,#13847,#13848,#13849,#13850,#13851,#13852,#13853,#13854,
#13855,#13856,#13857,#13858,#13859,#13860),.UNSPECIFIED.,.F.,.F.,(4,3,3,
3,3,3,3,4),(-104.379939320515,-103.838843045582,-102.840392631682,-101.841942217783,
-100.843491803883,-99.8450413899829,-98.8465909760831,-98.096754013335),
 .UNSPECIFIED.);
#1725=B_SPLINE_CURVE_WITH_KNOTS('',3,(#13865,#13866,#13867,#13868,#13869,
#13870,#13871,#13872,#13873,#13874,#13875,#13876,#13877,#13878,#13879,#13880,
#13881,#13882,#13883,#13884,#13885,#13886),.UNSPECIFIED.,.F.,.F.,(4,3,3,
3,3,3,3,4),(95.5573427486709,95.8512397343836,96.8496901482835,97.8481405621833,
98.8465909760831,99.8450413899829,100.843491803883,101.84052805585),
 .UNSPECIFIED.);
#1726=B_SPLINE_CURVE_WITH_KNOTS('',3,(#13887,#13888,#13889,#13890,#13891,
#13892,#13893,#13894,#13895,#13896,#13897,#13898,#13899,#13900,#13901,#13902,
#13903,#13904,#13905,#13906,#13907,#13908,#13909,#13910,#13911),
 .UNSPECIFIED.,.F.,.F.,(4,3,3,3,3,3,3,3,4),(-98.096754013335,-97.8481405621833,
-96.8496901482834,-95.8512397343836,-94.8527893204838,-93.854338906584,
-92.8558884926841,-91.8574380787843,-91.8135687061554),.UNSPECIFIED.);
#1727=B_SPLINE_CURVE_WITH_KNOTS('',3,(#13916,#13917,#13918,#13919,#13920,
#13921,#13922,#13923,#13924,#13925,#13926,#13927,#13928,#13929,#13930,#13931,
#13932,#13933,#13934,#13935,#13936,#13937),.UNSPECIFIED.,.F.,.F.,(4,3,3,
3,3,3,3,4),(89.2741574414913,89.8605372509847,90.8589876648845,91.8574380787843,
92.8558884926841,93.854338906584,94.8527893204838,95.5573427486709),
 .UNSPECIFIED.);
#1728=B_SPLINE_CURVE_WITH_KNOTS('',3,(#13938,#13939,#13940,#13941,#13942,
#13943,#13944,#13945,#13946,#13947,#13948,#13949,#13950,#13951,#13952,#13953,
#13954,#13955,#13956,#13957,#13958,#13959),.UNSPECIFIED.,.F.,.F.,(4,3,3,
3,3,3,3,4),(-91.8135687061554,-90.8589876648845,-89.8605372509847,-88.8620868370848,
-87.863636423185,-86.8651860092852,-85.8667355953853,-85.5303833989758),
 .UNSPECIFIED.);
#1729=B_SPLINE_CURVE_WITH_KNOTS('',3,(#13964,#13965,#13966,#13967,#13968,
#13969,#13970,#13971,#13972,#13973,#13974,#13975,#13976,#13977,#13978,#13979,
#13980,#13981,#13982,#13983,#13984,#13985),.UNSPECIFIED.,.F.,.F.,(4,3,3,
3,3,3,3,4),(82.9909721343117,83.8698347675857,84.8682851814855,85.8667355953854,
86.8651860092852,87.863636423185,88.8620868370848,89.2741574414913),
 .UNSPECIFIED.);
#1730=B_SPLINE_CURVE_WITH_KNOTS('',3,(#13986,#13987,#13988,#13989,#13990,
#13991,#13992,#13993,#13994,#13995,#13996,#13997,#13998,#13999,#14000,#14001,
#14002,#14003,#14004,#14005,#14006,#14007),.UNSPECIFIED.,.F.,.F.,(4,3,3,
3,3,3,3,4),(-85.5303833989758,-84.8682851814855,-83.8698347675857,-82.8713843536859,
-81.872933939786,-80.8744835258862,-79.8760331119863,-79.2471980917962),
 .UNSPECIFIED.);
#1731=B_SPLINE_CURVE_WITH_KNOTS('',3,(#14012,#14013,#14014,#14015,#14016,
#14017,#14018,#14019,#14020,#14021,#14022,#14023,#14024,#14025,#14026,#14027,
#14028,#14029,#14030,#14031,#14032,#14033,#14034,#14035,#14036),
 .UNSPECIFIED.,.F.,.F.,(4,3,3,3,3,3,3,3,4),(76.7077868271321,76.8806818702869,
77.8791322841867,78.8775826980865,79.8760331119864,80.8744835258862,81.872933939786,
82.8713843536859,82.9909721343117),.UNSPECIFIED.);
#1732=B_SPLINE_CURVE_WITH_KNOTS('',3,(#14037,#14038,#14039,#14040,#14041,
#14042,#14043,#14044,#14045,#14046,#14047,#14048,#14049,#14050,#14051,#14052,
#14053,#14054,#14055,#14056,#14057,#14058),.UNSPECIFIED.,.F.,.F.,(4,3,3,
3,3,3,3,4),(-79.2471980917962,-78.8775826980865,-77.8791322841867,-76.8806818702869,
-75.882231456387,-74.8837810424872,-73.8853306285874,-72.9640127846166),
 .UNSPECIFIED.);
#1733=B_SPLINE_CURVE_WITH_KNOTS('',3,(#14063,#14064,#14065,#14066,#14067,
#14068,#14069,#14070,#14071,#14072,#14073,#14074,#14075,#14076,#14077,#14078,
#14079,#14080,#14081,#14082,#14083,#14084),.UNSPECIFIED.,.F.,.F.,(4,3,3,
3,3,3,3,4),(70.4246015199525,70.8899793868879,71.8884298007877,72.8868802146876,
73.8853306285874,74.8837810424872,75.882231456387,76.7077868271321),
 .UNSPECIFIED.);
#1734=B_SPLINE_CURVE_WITH_KNOTS('',3,(#14085,#14086,#14087,#14088,#14089,
#14090,#14091,#14092,#14093,#14094,#14095,#14096,#14097,#14098,#14099,#14100,
#14101,#14102,#14103,#14104,#14105,#14106,#14107,#14108,#14109),
 .UNSPECIFIED.,.F.,.F.,(4,3,3,3,3,3,3,3,4),(-72.9640127846166,-72.8868802146875,
-71.8884298007877,-70.8899793868879,-69.891528972988,-68.8930785590882,
-67.8946281451884,-66.8961777312885,-66.680827477437),.UNSPECIFIED.);
#1735=B_SPLINE_CURVE_WITH_KNOTS('',3,(#14114,#14115,#14116,#14117,#14118,
#14119,#14120,#14121,#14122,#14123,#14124,#14125,#14126,#14127,#14128,#14129,
#14130,#14131,#14132,#14133,#14134,#14135),.UNSPECIFIED.,.F.,.F.,(4,3,3,
3,3,3,3,4),(64.1414162127729,64.8992769034889,65.8977273173887,66.8961777312886,
67.8946281451884,68.8930785590882,69.8915289729881,70.4246015199525),
 .UNSPECIFIED.);
#1736=B_SPLINE_CURVE_WITH_KNOTS('',3,(#14136,#14137,#14138,#14139,#14140,
#14141,#14142,#14143,#14144,#14145,#14146,#14147,#14148,#14149,#14150,#14151,
#14152,#14153,#14154,#14155,#14156,#14157),.UNSPECIFIED.,.F.,.F.,(4,3,3,
3,3,3,3,4),(-66.680827477437,-65.8977273173887,-64.8992769034889,-63.9008264895891,
-62.9023760756893,-61.9039256617894,-60.9054752478896,-60.3976421702574),
 .UNSPECIFIED.);
#1737=B_SPLINE_CURVE_WITH_KNOTS('',3,(#14162,#14163,#14164,#14165,#14166,
#14167,#14168,#14169,#14170,#14171,#14172,#14173,#14174,#14175,#14176,#14177,
#14178,#14179,#14180,#14181,#14182,#14183,#14184,#14185,#14186),
 .UNSPECIFIED.,.F.,.F.,(4,3,3,3,3,3,3,3,4),(57.8582309055933,57.9101240061901,
58.9085744200899,59.9070248339898,60.9054752478896,61.9039256617894,62.9023760756893,
63.9008264895891,64.1414162127729),.UNSPECIFIED.);
#1738=B_SPLINE_CURVE_WITH_KNOTS('',3,(#14187,#14188,#14189,#14190,#14191,
#14192,#14193,#14194,#14195,#14196,#14197,#14198,#14199,#14200,#14201,#14202,
#14203,#14204,#14205,#14206,#14207,#14208),.UNSPECIFIED.,.F.,.F.,(4,3,3,
3,3,3,3,4),(-60.3976421702574,-59.9070248339898,-58.9085744200899,-57.9101240061901,
-56.9116735922903,-55.9132231783905,-54.9147727644906,-54.1144568630778),
 .UNSPECIFIED.);
#1739=B_SPLINE_CURVE_WITH_KNOTS('',3,(#14213,#14214,#14215,#14216,#14217,
#14218,#14219,#14220,#14221,#14222,#14223,#14224,#14225,#14226,#14227,#14228,
#14229,#14230,#14231,#14232,#14233,#14234),.UNSPECIFIED.,.F.,.F.,(4,3,3,
3,3,3,3,4),(51.5750455984138,51.9194215227911,52.917871936691,53.9163223505908,
54.9147727644906,55.9132231783905,56.9116735922903,57.8582309055933),
 .UNSPECIFIED.);
#1740=B_SPLINE_CURVE_WITH_KNOTS('',3,(#14235,#14236,#14237,#14238,#14239,
#14240,#14241,#14242,#14243,#14244,#14245,#14246,#14247,#14248,#14249,#14250,
#14251,#14252,#14253,#14254,#14255,#14256,#14257,#14258,#14259),
 .UNSPECIFIED.,.F.,.F.,(4,3,3,3,3,3,3,3,4),(-54.1144568630778,-53.9163223505908,
-52.917871936691,-51.9194215227911,-50.9209711088913,-49.9225206949915,
-48.9240702810916,-47.9256198671918,-47.8312715558982),.UNSPECIFIED.);
#1741=B_SPLINE_CURVE_WITH_KNOTS('',3,(#14264,#14265,#14266,#14267,#14268,
#14269,#14270,#14271,#14272,#14273,#14274,#14275,#14276,#14277,#14278,#14279,
#14280,#14281,#14282,#14283,#14284,#14285),.UNSPECIFIED.,.F.,.F.,(4,3,3,
3,3,3,3,4),(45.2918602912342,45.9287190393922,46.927169453292,47.9256198671918,
48.9240702810917,49.9225206949915,50.9209711088913,51.5750455984138),
 .UNSPECIFIED.);
#1742=B_SPLINE_CURVE_WITH_KNOTS('',3,(#14286,#14287,#14288,#14289,#14290,
#14291,#14292,#14293,#14294,#14295,#14296,#14297,#14298,#14299,#14300,#14301,
#14302,#14303,#14304,#14305,#14306,#14307),.UNSPECIFIED.,.F.,.F.,(4,3,3,
3,3,3,3,4),(-47.8312715558982,-46.927169453292,-45.9287190393921,-44.9302686254923,
-43.9318182115925,-42.9333677976927,-41.9349173837928,-41.5480862487187),
 .UNSPECIFIED.);
#1743=B_SPLINE_CURVE_WITH_KNOTS('',3,(#14312,#14313,#14314,#14315,#14316,
#14317,#14318,#14319,#14320,#14321,#14322,#14323,#14324,#14325,#14326,#14327,
#14328,#14329,#14330,#14331,#14332,#14333),.UNSPECIFIED.,.F.,.F.,(4,3,3,
3,3,3,3,4),(39.0086749840546,39.9380165559932,40.936466969893,41.9349173837928,
42.9333677976927,43.9318182115925,44.9302686254923,45.2918602912342),
 .UNSPECIFIED.);
#1744=B_SPLINE_CURVE_WITH_KNOTS('',3,(#14334,#14335,#14336,#14337,#14338,
#14339,#14340,#14341,#14342,#14343,#14344,#14345,#14346,#14347,#14348,#14349,
#14350,#14351,#14352,#14353,#14354,#14355),.UNSPECIFIED.,.F.,.F.,(4,3,3,
3,3,3,3,4),(-41.5480862487187,-40.936466969893,-39.9380165559932,-38.9395661420933,
-37.9411157281935,-36.9426653142937,-35.9442149003939,-35.2649009415391),
 .UNSPECIFIED.);
#1745=B_SPLINE_CURVE_WITH_KNOTS('',3,(#14360,#14361,#14362,#14363,#14364,
#14365,#14366,#14367,#14368,#14369,#14370,#14371,#14372,#14373,#14374,#14375,
#14376,#14377,#14378,#14379,#14380,#14381,#14382,#14383,#14384),
 .UNSPECIFIED.,.F.,.F.,(4,3,3,3,3,3,3,3,4),(32.725489676875,32.9488636586944,
33.9473140725942,34.945764486494,35.9442149003939,36.9426653142937,37.9411157281935,
38.9395661420934,39.0086749840546),.UNSPECIFIED.);
#1746=B_SPLINE_CURVE_WITH_KNOTS('',3,(#14385,#14386,#14387,#14388,#14389,
#14390,#14391,#14392,#14393,#14394,#14395,#14396,#14397,#14398,#14399,#14400,
#14401,#14402,#14403,#14404,#14405,#14406),.UNSPECIFIED.,.F.,.F.,(4,3,3,
3,3,3,3,4),(-35.2649009415391,-34.945764486494,-33.9473140725942,-32.9488636586944,
-31.9504132447945,-30.9519628308947,-29.9535124169949,-28.9817156343595),
 .UNSPECIFIED.);
#1747=B_SPLINE_CURVE_WITH_KNOTS('',3,(#14411,#14412,#14413,#14414,#14415,
#14416,#14417,#14418,#14419,#14420,#14421,#14422,#14423,#14424,#14425,#14426,
#14427,#14428,#14429,#14430,#14431,#14432),.UNSPECIFIED.,.F.,.F.,(4,3,3,
3,3,3,3,4),(26.4423043696954,26.9581611752954,27.9566115891952,28.9550620030951,
29.9535124169949,30.9519628308947,31.9504132447945,32.725489676875),
 .UNSPECIFIED.);
#1748=B_SPLINE_CURVE_WITH_KNOTS('',3,(#14433,#14434,#14435,#14436,#14437,
#14438,#14439,#14440,#14441,#14442,#14443,#14444,#14445,#14446,#14447,#14448,
#14449,#14450,#14451,#14452,#14453,#14454,#14455,#14456,#14457),
 .UNSPECIFIED.,.F.,.F.,(4,3,3,3,3,3,3,3,4),(-28.9817156343595,-28.955062003095,
-27.9566115891952,-26.9581611752954,-25.9597107613956,-24.9612603474957,
-23.9628099335959,-22.9643595196961,-22.6985303271799),.UNSPECIFIED.);
#1749=B_SPLINE_CURVE_WITH_KNOTS('',3,(#14462,#14463,#14464,#14465,#14466,
#14467,#14468,#14469,#14470,#14471,#14472,#14473,#14474,#14475,#14476,#14477,
#14478,#14479,#14480,#14481,#14482,#14483),.UNSPECIFIED.,.F.,.F.,(4,3,3,
3,3,3,3,4),(20.1591190625158,20.9674586918964,21.9659091057962,22.9643595196961,
23.9628099335959,24.9612603474957,25.9597107613956,26.4423043696954),
 .UNSPECIFIED.);
#1750=B_SPLINE_CURVE_WITH_KNOTS('',3,(#14484,#14485,#14486,#14487,#14488,
#14489,#14490,#14491,#14492,#14493,#14494,#14495,#14496,#14497,#14498,#14499,
#14500,#14501,#14502,#14503,#14504,#14505),.UNSPECIFIED.,.F.,.F.,(4,3,3,
3,3,3,3,4),(-22.6985303271799,-21.9659091057962,-20.9674586918964,-19.9690082779966,
-18.9705578640968,-17.9721074501969,-16.9736570362971,-16.4153450200003),
 .UNSPECIFIED.);
#1751=B_SPLINE_CURVE_WITH_KNOTS('',3,(#14510,#14511,#14512,#14513,#14514,
#14515,#14516,#14517,#14518,#14519,#14520,#14521,#14522,#14523,#14524,#14525,
#14526,#14527,#14528,#14529,#14530,#14531,#14532,#14533,#14534),
 .UNSPECIFIED.,.F.,.F.,(4,3,3,3,3,3,3,3,4),(13.8759337553362,13.9783057945976,
14.9767562084974,15.9752066223973,16.9736570362971,17.9721074501969,18.9705578640968,
19.9690082779966,20.1591190625158),.UNSPECIFIED.);
#1752=B_SPLINE_CURVE_WITH_KNOTS('',3,(#14535,#14536,#14537,#14538,#14539,
#14540,#14541,#14542,#14543,#14544,#14545,#14546,#14547,#14548,#14549,#14550,
#14551,#14552,#14553,#14554,#14555,#14556),.UNSPECIFIED.,.F.,.F.,(4,3,3,
3,3,3,3,4),(-16.4153450200003,-15.9752066223973,-14.9767562084974,-13.9783057945976,
-12.9798553806978,-11.9814049667979,-10.9829545528981,-10.1321597128207),
 .UNSPECIFIED.);
#1753=B_SPLINE_CURVE_WITH_KNOTS('',3,(#14562,#14563,#14564,#14565,#14566,
#14567,#14568,#14569,#14570,#14571,#14572,#14573,#14574),.UNSPECIFIED.,
 .F.,.F.,(4,3,3,3,4),(-3.84897440564114,-2.99535124169949,-1.99690082779966,
-0.99845041389983,0.),.UNSPECIFIED.);
#1754=B_SPLINE_CURVE_WITH_KNOTS('',3,(#14577,#14578,#14579,#14580,#14581,
#14582,#14583,#14584,#14585,#14586,#14587,#14588,#14589,#14590,#14591,#14592,
#14593,#14594,#14595),.UNSPECIFIED.,.F.,.F.,(4,3,3,3,3,3,4),(2.01694489302824,
2.99535124169949,3.99380165559932,4.99225206949915,5.99070248339898,6.98915289729881,
7.59274844815663),.UNSPECIFIED.);
#1755=B_SPLINE_CURVE_WITH_KNOTS('',3,(#14601,#14602,#14603,#14604,#14605,
#14606,#14607,#14608),.UNSPECIFIED.,.F.,.F.,(4,1,1,1,1,4),(116.238928182822,
116.69628232179,117.69473273569,118.693183149589,119.691633563489,120.690083977389),
 .UNSPECIFIED.);
#1756=B_SPLINE_CURVE_WITH_KNOTS('',3,(#14611,#14612,#14613,#14614,#14615,
#14616,#14617,#14618,#14619),.UNSPECIFIED.,.F.,.F.,(4,1,1,1,1,1,4),(116.238928182822,
116.240342344754,117.238792758654,118.237243172554,119.235693586454,120.234144000354,
121.212550349025),.UNSPECIFIED.);
#1757=B_SPLINE_CURVE_WITH_KNOTS('',3,(#14624,#14625,#14626,#14627,#14628,
#14629,#14630,#14631,#14632,#14633),.UNSPECIFIED.,.F.,.F.,(4,1,1,1,1,1,
1,4),(109.955742875643,110.705579838391,111.704030252291,112.70248066619,
113.70093108009,114.69938149399,115.69783190789,116.238928182822),
 .UNSPECIFIED.);
#1758=B_SPLINE_CURVE_WITH_KNOTS('',3,(#14634,#14635,#14636,#14637,#14638,
#14639,#14640,#14641,#14642,#14643),.UNSPECIFIED.,.F.,.F.,(4,1,1,1,1,1,
1,4),(109.955742875643,110.249639861355,111.248090275255,112.246540689155,
113.244991103055,114.243441516955,115.241891930855,116.238928182822),
 .UNSPECIFIED.);
#1759=B_SPLINE_CURVE_WITH_KNOTS('',3,(#14648,#14649,#14650,#14651,#14652,
#14653,#14654,#14655,#14656,#14657,#14658),.UNSPECIFIED.,.F.,.F.,(4,1,1,
1,1,1,1,1,4),(103.672557568463,103.716426941092,104.714877354992,105.713327768892,
106.711778182792,107.710228596691,108.708679010591,109.707129424491,109.955742875643),
 .UNSPECIFIED.);
#1760=B_SPLINE_CURVE_WITH_KNOTS('',3,(#14659,#14660,#14661,#14662,#14663,
#14664,#14665,#14666,#14667,#14668),.UNSPECIFIED.,.F.,.F.,(4,1,1,1,1,1,
1,4),(103.672557568463,104.258937377956,105.257387791856,106.255838205756,
107.254288619656,108.252739033556,109.251189447456,109.955742875643),
 .UNSPECIFIED.);
#1761=B_SPLINE_CURVE_WITH_KNOTS('',3,(#14673,#14674,#14675,#14676,#14677,
#14678,#14679,#14680,#14681,#14682),.UNSPECIFIED.,.F.,.F.,(4,1,1,1,1,1,
1,4),(97.3893722612835,97.725724457693,98.7241748715929,99.7226252854927,
100.721075699393,101.719526113292,102.717976527192,103.672557568463),
 .UNSPECIFIED.);
#1762=B_SPLINE_CURVE_WITH_KNOTS('',3,(#14683,#14684,#14685,#14686,#14687,
#14688,#14689,#14690,#14691,#14692),.UNSPECIFIED.,.F.,.F.,(4,1,1,1,1,1,
1,4),(97.3893722612835,98.2682348945574,99.2666853084572,100.265135722357,
101.263586136257,102.262036550157,103.260486964057,103.672557568463),
 .UNSPECIFIED.);
#1763=B_SPLINE_CURVE_WITH_KNOTS('',3,(#14697,#14698,#14699,#14700,#14701,
#14702,#14703,#14704,#14705,#14706),.UNSPECIFIED.,.F.,.F.,(4,1,1,1,1,1,
1,4),(91.106186954104,91.7350219742941,92.7334723881939,93.7319228020937,
94.7303732159936,95.7288236298934,96.7272740437932,97.3893722612835),
 .UNSPECIFIED.);
#1764=B_SPLINE_CURVE_WITH_KNOTS('',3,(#14707,#14708,#14709,#14710,#14711,
#14712,#14713,#14714,#14715,#14716,#14717),.UNSPECIFIED.,.F.,.F.,(4,1,1,
1,1,1,1,1,4),(91.106186954104,91.2790819972586,92.2775324111584,93.2759828250583,
94.2744332389581,95.2728836528579,96.2713340667578,97.2697844806576,97.3893722612835),
 .UNSPECIFIED.);
#1765=B_SPLINE_CURVE_WITH_KNOTS('',3,(#14722,#14723,#14724,#14725,#14726,
#14727,#14728,#14729,#14730,#14731),.UNSPECIFIED.,.F.,.F.,(4,1,1,1,1,1,
1,4),(84.8230016469244,85.7443194908951,86.7427699047949,87.7412203186948,
88.7396707325946,89.7381211464944,90.7365715603942,91.106186954104),
 .UNSPECIFIED.);
#1766=B_SPLINE_CURVE_WITH_KNOTS('',3,(#14732,#14733,#14734,#14735,#14736,
#14737,#14738,#14739,#14740,#14741),.UNSPECIFIED.,.F.,.F.,(4,1,1,1,1,1,
1,4),(84.8230016469244,85.2883795138596,86.2868299277595,87.2852803416593,
88.2837307555591,89.282181169459,90.2806315833588,91.106186954104),
 .UNSPECIFIED.);
#1767=B_SPLINE_CURVE_WITH_KNOTS('',3,(#14746,#14747,#14748,#14749,#14750,
#14751,#14752,#14753,#14754,#14755,#14756),.UNSPECIFIED.,.F.,.F.,(4,1,1,
1,1,1,1,1,4),(78.5398163397448,78.7551665935963,79.7536170074961,80.7520674213959,
81.7505178352958,82.7489682491956,83.7474186630954,84.7458690769953,84.8230016469244),
 .UNSPECIFIED.);
#1768=B_SPLINE_CURVE_WITH_KNOTS('',3,(#14757,#14758,#14759,#14760,#14761,
#14762,#14763,#14764,#14765,#14766),.UNSPECIFIED.,.F.,.F.,(4,1,1,1,1,1,
1,4),(78.5398163397448,79.2976770304607,80.2961274443605,81.2945778582603,
82.2930282721601,83.29147868606,84.2899290999598,84.8230016469244),
 .UNSPECIFIED.);
#1769=B_SPLINE_CURVE_WITH_KNOTS('',3,(#14771,#14772,#14773,#14774,#14775,
#14776,#14777,#14778,#14779,#14780),.UNSPECIFIED.,.F.,.F.,(4,1,1,1,1,1,
1,4),(72.2566310325652,72.7644641101973,73.7629145240971,74.761364937997,
75.7598153518968,76.7582657657966,77.7567161796965,78.5398163397448),
 .UNSPECIFIED.);
#1770=B_SPLINE_CURVE_WITH_KNOTS('',3,(#14781,#14782,#14783,#14784,#14785,
#14786,#14787,#14788,#14789,#14790,#14791),.UNSPECIFIED.,.F.,.F.,(4,1,1,
1,1,1,1,1,4),(72.2566310325652,72.3085241331619,73.3069745470617,74.3054249609615,
75.3038753748613,76.3023257887612,77.300776202661,78.2992266165608,78.5398163397448),
 .UNSPECIFIED.);
#1771=B_SPLINE_CURVE_WITH_KNOTS('',3,(#14796,#14797,#14798,#14799,#14800,
#14801,#14802,#14803,#14804,#14805),.UNSPECIFIED.,.F.,.F.,(4,1,1,1,1,1,
1,4),(65.9734457253856,66.7737616267983,67.7722120406982,68.770662454598,
69.7691128684978,70.7675632823977,71.7660136962975,72.2566310325652),
 .UNSPECIFIED.);
#1772=B_SPLINE_CURVE_WITH_KNOTS('',3,(#14806,#14807,#14808,#14809,#14810,
#14811,#14812,#14813,#14814,#14815),.UNSPECIFIED.,.F.,.F.,(4,1,1,1,1,1,
1,4),(65.9734457253856,66.3178216497629,67.3162720636627,68.3147224775625,
69.3131728914624,70.3116233053622,71.310073719262,72.2566310325652),
 .UNSPECIFIED.);
#1773=B_SPLINE_CURVE_WITH_KNOTS('',3,(#14820,#14821,#14822,#14823,#14824,
#14825,#14826,#14827,#14828,#14829,#14830),.UNSPECIFIED.,.F.,.F.,(4,1,1,
1,1,1,1,1,4),(59.690260418206,59.7846087294995,60.7830591433994,61.7815095572992,
62.779959971199,63.7784103850989,64.7768607989987,65.7753112128985,65.9734457253856),
 .UNSPECIFIED.);
#1774=B_SPLINE_CURVE_WITH_KNOTS('',3,(#14831,#14832,#14833,#14834,#14835,
#14836,#14837,#14838,#14839,#14840),.UNSPECIFIED.,.F.,.F.,(4,1,1,1,1,1,
1,4),(59.690260418206,60.3271191663639,61.3255695802637,62.3240199941636,
63.3224704080634,64.3209208219632,65.319371235863,65.9734457253856),
 .UNSPECIFIED.);
#1775=B_SPLINE_CURVE_WITH_KNOTS('',3,(#14845,#14846,#14847,#14848,#14849,
#14850,#14851,#14852,#14853,#14854),.UNSPECIFIED.,.F.,.F.,(4,1,1,1,1,1,
1,4),(53.4070751110264,53.7939062461006,54.7923566600004,55.7908070739002,
56.7892574878001,57.7877079016999,58.7861583155997,59.690260418206),
 .UNSPECIFIED.);
#1776=B_SPLINE_CURVE_WITH_KNOTS('',3,(#14855,#14856,#14857,#14858,#14859,
#14860,#14861,#14862,#14863,#14864),.UNSPECIFIED.,.F.,.F.,(4,1,1,1,1,1,
1,4),(53.4070751110264,54.3364166829649,55.3348670968648,56.3333175107646,
57.3317679246644,58.3302183385642,59.3286687524641,59.690260418206),
 .UNSPECIFIED.);
#1777=B_SPLINE_CURVE_WITH_KNOTS('',3,(#14869,#14870,#14871,#14872,#14873,
#14874,#14875,#14876,#14877,#14878),.UNSPECIFIED.,.F.,.F.,(4,1,1,1,1,1,
1,4),(47.1238898038468,47.8032037627016,48.8016541766014,49.8001045905012,
50.7985550044011,51.7970054183009,52.7954558322007,53.4070751110264),
 .UNSPECIFIED.);
#1778=B_SPLINE_CURVE_WITH_KNOTS('',3,(#14879,#14880,#14881,#14882,#14883,
#14884,#14885,#14886,#14887,#14888,#14889),.UNSPECIFIED.,.F.,.F.,(4,1,1,
1,1,1,1,1,4),(47.1238898038468,47.3472637856661,48.3457141995659,49.3441646134658,
50.3426150273656,51.3410654412654,52.3395158551653,53.3379662690651,53.4070751110264),
 .UNSPECIFIED.);
#1779=B_SPLINE_CURVE_WITH_KNOTS('',3,(#14894,#14895,#14896,#14897,#14898,
#14899,#14900,#14901,#14902,#14903),.UNSPECIFIED.,.F.,.F.,(4,1,1,1,1,1,
1,4),(40.8407044966672,41.8125012793026,42.8109516932024,43.8094021071023,
44.8078525210021,45.8063029349019,46.8047533488018,47.1238898038468),
 .UNSPECIFIED.);
#1780=B_SPLINE_CURVE_WITH_KNOTS('',3,(#14904,#14905,#14906,#14907,#14908,
#14909,#14910,#14911,#14912,#14913),.UNSPECIFIED.,.F.,.F.,(4,1,1,1,1,1,
1,4),(40.8407044966672,41.3565613022671,42.355011716167,43.3534621300668,
44.3519125439666,45.3503629578665,46.3488133717663,47.1238898038468),
 .UNSPECIFIED.);
#1781=B_SPLINE_CURVE_WITH_KNOTS('',3,(#14918,#14919,#14920,#14921,#14922,
#14923,#14924,#14925,#14926,#14927,#14928),.UNSPECIFIED.,.F.,.F.,(4,1,1,
1,1,1,1,1,4),(34.5575191894876,34.8233483820038,35.8217987959036,36.8202492098035,
37.8186996237033,38.8171500376031,39.8156004515029,40.8140508654028,40.8407044966672),
 .UNSPECIFIED.);
#1782=B_SPLINE_CURVE_WITH_KNOTS('',3,(#14929,#14930,#14931,#14932,#14933,
#14934,#14935,#14936,#14937,#14938),.UNSPECIFIED.,.F.,.F.,(4,1,1,1,1,1,
1,4),(34.5575191894876,35.3658588188682,36.364309232768,37.3627596466678,
38.3612100605677,39.3596604744675,40.3581108883673,40.8407044966672),
 .UNSPECIFIED.);
#1783=B_SPLINE_CURVE_WITH_KNOTS('',3,(#14943,#14944,#14945,#14946,#14947,
#14948,#14949,#14950,#14951,#14952),.UNSPECIFIED.,.F.,.F.,(4,1,1,1,1,1,
1,4),(28.274333882308,28.8326458986048,29.8310963125047,30.8295467264045,
31.8279971403043,32.8264475542041,33.824897968104,34.5575191894876),
 .UNSPECIFIED.);
#1784=B_SPLINE_CURVE_WITH_KNOTS('',3,(#14953,#14954,#14955,#14956,#14957,
#14958,#14959,#14960,#14961,#14962,#14963),.UNSPECIFIED.,.F.,.F.,(4,1,1,
1,1,1,1,1,4),(28.274333882308,28.3767059215694,29.3751563354692,30.373606749369,
31.3720571632688,32.3705075771687,33.3689579910685,34.3674084049683,34.5575191894876),
 .UNSPECIFIED.);
#1785=B_SPLINE_CURVE_WITH_KNOTS('',3,(#14968,#14969,#14970,#14971,#14972,
#14973,#14974,#14975,#14976,#14977),.UNSPECIFIED.,.F.,.F.,(4,1,1,1,1,1,
1,4),(21.9911485751285,22.8419434152058,23.8403938291057,24.8388442430055,
25.8372946569053,26.8357450708052,27.834195484705,28.274333882308),
 .UNSPECIFIED.);
#1786=B_SPLINE_CURVE_WITH_KNOTS('',3,(#14978,#14979,#14980,#14981,#14982,
#14983,#14984,#14985,#14986,#14987),.UNSPECIFIED.,.F.,.F.,(4,1,1,1,1,1,
1,4),(21.9911485751284,22.3860034381704,23.3844538520702,24.38290426597,
25.3813546798699,26.3798050937697,27.3782555076695,28.274333882308),
 .UNSPECIFIED.);
#1787=B_SPLINE_CURVE_WITH_KNOTS('',3,(#14993,#14994,#14995,#14996,#14997),
 .UNSPECIFIED.,.F.,.F.,(4,1,4),(14.3984001269718,15.3968505408716,15.7079632679489),
 .UNSPECIFIED.);
#1788=B_SPLINE_CURVE_WITH_KNOTS('',3,(#15000,#15001,#15002,#15003,#15004),
 .UNSPECIFIED.,.F.,.F.,(4,1,4),(13.8759337553362,14.8543401040072,15.7079632679489),
 .UNSPECIFIED.);
#1789=B_SPLINE_CURVE_WITH_KNOTS('',3,(#15010,#15011,#15012,#15013),
 .UNSPECIFIED.,.F.,.F.,(4,4),(108.12371336303,108.831095115081),
 .UNSPECIFIED.);
#1790=B_SPLINE_CURVE_WITH_KNOTS('',3,(#15021,#15022,#15023,#15024,#15025,
#15026,#15027,#15028,#15029,#15030),.UNSPECIFIED.,.F.,.F.,(4,3,3,4),(-106.814150222053,
-105.835743873382,-104.837293459482,-104.379939320515),.UNSPECIFIED.);
#1791=B_SPLINE_CURVE_WITH_KNOTS('',3,(#15035,#15036,#15037,#15038,#15039,
#15040,#15041,#15042,#15043,#15044,#15045,#15046,#15047,#15048,#15049,#15050,
#15051,#15052,#15053,#15054,#15055,#15056),.UNSPECIFIED.,.F.,.F.,(4,3,3,
3,3,3,3,4),(101.84052805585,102.840392631682,103.838843045582,104.837293459482,
105.835743873382,106.834194287282,107.832644701182,108.12371336303),
 .UNSPECIFIED.);
#1792=B_SPLINE_CURVE_WITH_KNOTS('',3,(#15057,#15058,#15059,#15060,#15061,
#15062,#15063,#15064,#15065,#15066,#15067,#15068,#15069,#15070,#15071,#15072,
#15073,#15074,#15075,#15076,#15077,#15078),.UNSPECIFIED.,.F.,.F.,(4,3,3,
3,3,3,3,4),(-104.379939320515,-103.838843045582,-102.840392631682,-101.841942217783,
-100.843491803883,-99.8450413899829,-98.8465909760831,-98.096754013335),
 .UNSPECIFIED.);
#1793=B_SPLINE_CURVE_WITH_KNOTS('',3,(#15083,#15084,#15085,#15086,#15087,
#15088,#15089,#15090,#15091,#15092,#15093,#15094,#15095,#15096,#15097,#15098,
#15099,#15100,#15101,#15102,#15103,#15104),.UNSPECIFIED.,.F.,.F.,(4,3,3,
3,3,3,3,4),(95.5573427486709,95.8512397343836,96.8496901482834,97.8481405621833,
98.8465909760831,99.8450413899829,100.843491803883,101.84052805585),
 .UNSPECIFIED.);
#1794=B_SPLINE_CURVE_WITH_KNOTS('',3,(#15105,#15106,#15107,#15108,#15109,
#15110,#15111,#15112,#15113,#15114,#15115,#15116,#15117,#15118,#15119,#15120,
#15121,#15122,#15123,#15124,#15125,#15126,#15127,#15128,#15129),
 .UNSPECIFIED.,.F.,.F.,(4,3,3,3,3,3,3,3,4),(-98.096754013335,-97.8481405621833,
-96.8496901482835,-95.8512397343836,-94.8527893204838,-93.854338906584,
-92.8558884926841,-91.8574380787843,-91.8135687061554),.UNSPECIFIED.);
#1795=B_SPLINE_CURVE_WITH_KNOTS('',3,(#15134,#15135,#15136,#15137,#15138,
#15139,#15140,#15141,#15142,#15143,#15144,#15145,#15146,#15147,#15148,#15149,
#15150,#15151,#15152,#15153,#15154,#15155),.UNSPECIFIED.,.F.,.F.,(4,3,3,
3,3,3,3,4),(89.2741574414913,89.8605372509846,90.8589876648845,91.8574380787843,
92.8558884926841,93.854338906584,94.8527893204838,95.5573427486709),
 .UNSPECIFIED.);
#1796=B_SPLINE_CURVE_WITH_KNOTS('',3,(#15156,#15157,#15158,#15159,#15160,
#15161,#15162,#15163,#15164,#15165,#15166,#15167,#15168,#15169,#15170,#15171,
#15172,#15173,#15174,#15175,#15176,#15177),.UNSPECIFIED.,.F.,.F.,(4,3,3,
3,3,3,3,4),(-91.8135687061554,-90.8589876648845,-89.8605372509847,-88.8620868370848,
-87.863636423185,-86.8651860092852,-85.8667355953854,-85.5303833989758),
 .UNSPECIFIED.);
#1797=B_SPLINE_CURVE_WITH_KNOTS('',3,(#15182,#15183,#15184,#15185,#15186,
#15187,#15188,#15189,#15190,#15191,#15192,#15193,#15194,#15195,#15196,#15197,
#15198,#15199,#15200,#15201,#15202,#15203),.UNSPECIFIED.,.F.,.F.,(4,3,3,
3,3,3,3,4),(82.9909721343117,83.8698347675857,84.8682851814855,85.8667355953853,
86.8651860092852,87.863636423185,88.8620868370848,89.2741574414913),
 .UNSPECIFIED.);
#1798=B_SPLINE_CURVE_WITH_KNOTS('',3,(#15204,#15205,#15206,#15207,#15208,
#15209,#15210,#15211,#15212,#15213,#15214,#15215,#15216,#15217,#15218,#15219,
#15220,#15221,#15222,#15223,#15224,#15225),.UNSPECIFIED.,.F.,.F.,(4,3,3,
3,3,3,3,4),(-85.5303833989758,-84.8682851814855,-83.8698347675857,-82.8713843536859,
-81.872933939786,-80.8744835258862,-79.8760331119864,-79.2471980917962),
 .UNSPECIFIED.);
#1799=B_SPLINE_CURVE_WITH_KNOTS('',3,(#15230,#15231,#15232,#15233,#15234,
#15235,#15236,#15237,#15238,#15239,#15240,#15241,#15242,#15243,#15244,#15245,
#15246,#15247,#15248,#15249,#15250,#15251,#15252,#15253,#15254),
 .UNSPECIFIED.,.F.,.F.,(4,3,3,3,3,3,3,3,4),(76.7077868271321,76.8806818702868,
77.8791322841867,78.8775826980865,79.8760331119864,80.8744835258862,81.872933939786,
82.8713843536859,82.9909721343117),.UNSPECIFIED.);
#1800=B_SPLINE_CURVE_WITH_KNOTS('',3,(#15255,#15256,#15257,#15258,#15259,
#15260,#15261,#15262,#15263,#15264,#15265,#15266,#15267,#15268,#15269,#15270,
#15271,#15272,#15273,#15274,#15275,#15276),.UNSPECIFIED.,.F.,.F.,(4,3,3,
3,3,3,3,4),(-79.2471980917962,-78.8775826980865,-77.8791322841867,-76.8806818702869,
-75.882231456387,-74.8837810424872,-73.8853306285874,-72.9640127846166),
 .UNSPECIFIED.);
#1801=B_SPLINE_CURVE_WITH_KNOTS('',3,(#15281,#15282,#15283,#15284,#15285,
#15286,#15287,#15288,#15289,#15290,#15291,#15292,#15293,#15294,#15295,#15296,
#15297,#15298,#15299,#15300,#15301,#15302),.UNSPECIFIED.,.F.,.F.,(4,3,3,
3,3,3,3,4),(70.4246015199525,70.8899793868879,71.8884298007877,72.8868802146875,
73.8853306285874,74.8837810424872,75.882231456387,76.7077868271321),
 .UNSPECIFIED.);
#1802=B_SPLINE_CURVE_WITH_KNOTS('',3,(#15303,#15304,#15305,#15306,#15307,
#15308,#15309,#15310,#15311,#15312,#15313,#15314,#15315,#15316,#15317,#15318,
#15319,#15320,#15321,#15322,#15323,#15324,#15325,#15326,#15327),
 .UNSPECIFIED.,.F.,.F.,(4,3,3,3,3,3,3,3,4),(-72.9640127846166,-72.8868802146875,
-71.8884298007877,-70.8899793868879,-69.891528972988,-68.8930785590882,
-67.8946281451884,-66.8961777312886,-66.680827477437),.UNSPECIFIED.);
#1803=B_SPLINE_CURVE_WITH_KNOTS('',3,(#15332,#15333,#15334,#15335,#15336,
#15337,#15338,#15339,#15340,#15341,#15342,#15343,#15344,#15345,#15346,#15347,
#15348,#15349,#15350,#15351,#15352,#15353),.UNSPECIFIED.,.F.,.F.,(4,3,3,
3,3,3,3,4),(64.1414162127729,64.8992769034889,65.8977273173887,66.8961777312886,
67.8946281451884,68.8930785590882,69.8915289729881,70.4246015199525),
 .UNSPECIFIED.);
#1804=B_SPLINE_CURVE_WITH_KNOTS('',3,(#15354,#15355,#15356,#15357,#15358,
#15359,#15360,#15361,#15362,#15363,#15364,#15365,#15366,#15367,#15368,#15369,
#15370,#15371,#15372,#15373,#15374,#15375),.UNSPECIFIED.,.F.,.F.,(4,3,3,
3,3,3,3,4),(-66.680827477437,-65.8977273173887,-64.8992769034889,-63.9008264895891,
-62.9023760756892,-61.9039256617894,-60.9054752478896,-60.3976421702575),
 .UNSPECIFIED.);
#1805=B_SPLINE_CURVE_WITH_KNOTS('',3,(#15380,#15381,#15382,#15383,#15384,
#15385,#15386,#15387,#15388,#15389,#15390,#15391,#15392,#15393,#15394,#15395,
#15396,#15397,#15398,#15399,#15400,#15401,#15402,#15403,#15404),
 .UNSPECIFIED.,.F.,.F.,(4,3,3,3,3,3,3,3,4),(57.8582309055933,57.9101240061901,
58.9085744200899,59.9070248339898,60.9054752478896,61.9039256617894,62.9023760756892,
63.9008264895891,64.1414162127729),.UNSPECIFIED.);
#1806=B_SPLINE_CURVE_WITH_KNOTS('',3,(#15405,#15406,#15407,#15408,#15409,
#15410,#15411,#15412,#15413,#15414,#15415,#15416,#15417,#15418,#15419,#15420,
#15421,#15422,#15423,#15424,#15425,#15426),.UNSPECIFIED.,.F.,.F.,(4,3,3,
3,3,3,3,4),(-60.3976421702575,-59.9070248339898,-58.9085744200899,-57.9101240061901,
-56.9116735922903,-55.9132231783904,-54.9147727644906,-54.1144568630779),
 .UNSPECIFIED.);
#1807=B_SPLINE_CURVE_WITH_KNOTS('',3,(#15431,#15432,#15433,#15434,#15435,
#15436,#15437,#15438,#15439,#15440,#15441,#15442,#15443,#15444,#15445,#15446,
#15447,#15448,#15449,#15450,#15451,#15452),.UNSPECIFIED.,.F.,.F.,(4,3,3,
3,3,3,3,4),(51.5750455984137,51.9194215227911,52.917871936691,53.9163223505908,
54.9147727644906,55.9132231783904,56.9116735922903,57.8582309055933),
 .UNSPECIFIED.);
#1808=B_SPLINE_CURVE_WITH_KNOTS('',3,(#15453,#15454,#15455,#15456,#15457,
#15458,#15459,#15460,#15461,#15462,#15463,#15464,#15465,#15466,#15467,#15468,
#15469,#15470,#15471,#15472,#15473,#15474,#15475,#15476,#15477),
 .UNSPECIFIED.,.F.,.F.,(4,3,3,3,3,3,3,3,4),(-54.1144568630779,-53.9163223505908,
-52.917871936691,-51.9194215227911,-50.9209711088913,-49.9225206949915,
-48.9240702810916,-47.9256198671918,-47.8312715558983),.UNSPECIFIED.);
#1809=B_SPLINE_CURVE_WITH_KNOTS('',3,(#15482,#15483,#15484,#15485,#15486,
#15487,#15488,#15489,#15490,#15491,#15492,#15493,#15494,#15495,#15496,#15497,
#15498,#15499,#15500,#15501,#15502,#15503),.UNSPECIFIED.,.F.,.F.,(4,3,3,
3,3,3,3,4),(45.2918602912341,45.9287190393921,46.927169453292,47.9256198671918,
48.9240702810916,49.9225206949915,50.9209711088913,51.5750455984137),
 .UNSPECIFIED.);
#1810=B_SPLINE_CURVE_WITH_KNOTS('',3,(#15504,#15505,#15506,#15507,#15508,
#15509,#15510,#15511,#15512,#15513,#15514,#15515,#15516,#15517,#15518,#15519,
#15520,#15521,#15522,#15523,#15524,#15525),.UNSPECIFIED.,.F.,.F.,(4,3,3,
3,3,3,3,4),(-47.8312715558983,-46.927169453292,-45.9287190393921,-44.9302686254923,
-43.9318182115925,-42.9333677976927,-41.9349173837928,-41.5480862487187),
 .UNSPECIFIED.);
#1811=B_SPLINE_CURVE_WITH_KNOTS('',3,(#15530,#15531,#15532,#15533,#15534,
#15535,#15536,#15537,#15538,#15539,#15540,#15541,#15542,#15543,#15544,#15545,
#15546,#15547,#15548,#15549,#15550,#15551),.UNSPECIFIED.,.F.,.F.,(4,3,3,
3,3,3,3,4),(39.0086749840546,39.9380165559932,40.936466969893,41.9349173837928,
42.9333677976927,43.9318182115925,44.9302686254923,45.2918602912341),
 .UNSPECIFIED.);
#1812=B_SPLINE_CURVE_WITH_KNOTS('',3,(#15552,#15553,#15554,#15555,#15556,
#15557,#15558,#15559,#15560,#15561,#15562,#15563,#15564,#15565,#15566,#15567,
#15568,#15569,#15570,#15571,#15572,#15573),.UNSPECIFIED.,.F.,.F.,(4,3,3,
3,3,3,3,4),(-41.5480862487187,-40.936466969893,-39.9380165559932,-38.9395661420933,
-37.9411157281935,-36.9426653142937,-35.9442149003939,-35.2649009415391),
 .UNSPECIFIED.);
#1813=B_SPLINE_CURVE_WITH_KNOTS('',3,(#15578,#15579,#15580,#15581,#15582,
#15583,#15584,#15585,#15586,#15587,#15588,#15589,#15590,#15591,#15592,#15593,
#15594,#15595,#15596,#15597,#15598,#15599,#15600,#15601,#15602),
 .UNSPECIFIED.,.F.,.F.,(4,3,3,3,3,3,3,3,4),(32.725489676875,32.9488636586944,
33.9473140725942,34.945764486494,35.9442149003939,36.9426653142937,37.9411157281935,
38.9395661420933,39.0086749840546),.UNSPECIFIED.);
#1814=B_SPLINE_CURVE_WITH_KNOTS('',3,(#15603,#15604,#15605,#15606,#15607,
#15608,#15609,#15610,#15611,#15612,#15613,#15614,#15615,#15616,#15617,#15618,
#15619,#15620,#15621,#15622,#15623,#15624),.UNSPECIFIED.,.F.,.F.,(4,3,3,
3,3,3,3,4),(-35.2649009415391,-34.945764486494,-33.9473140725942,-32.9488636586944,
-31.9504132447945,-30.9519628308947,-29.9535124169949,-28.9817156343595),
 .UNSPECIFIED.);
#1815=B_SPLINE_CURVE_WITH_KNOTS('',3,(#15629,#15630,#15631,#15632,#15633,
#15634,#15635,#15636,#15637,#15638,#15639,#15640,#15641,#15642,#15643,#15644,
#15645,#15646,#15647,#15648,#15649,#15650),.UNSPECIFIED.,.F.,.F.,(4,3,3,
3,3,3,3,4),(26.4423043696954,26.9581611752954,27.9566115891952,28.955062003095,
29.9535124169949,30.9519628308947,31.9504132447945,32.725489676875),
 .UNSPECIFIED.);
#1816=B_SPLINE_CURVE_WITH_KNOTS('',3,(#15651,#15652,#15653,#15654,#15655,
#15656,#15657,#15658,#15659,#15660,#15661,#15662,#15663,#15664,#15665,#15666,
#15667,#15668,#15669,#15670,#15671,#15672,#15673,#15674,#15675),
 .UNSPECIFIED.,.F.,.F.,(4,3,3,3,3,3,3,3,4),(-28.9817156343595,-28.955062003095,
-27.9566115891952,-26.9581611752954,-25.9597107613956,-24.9612603474957,
-23.9628099335959,-22.9643595196961,-22.6985303271799),.UNSPECIFIED.);
#1817=B_SPLINE_CURVE_WITH_KNOTS('',3,(#15680,#15681,#15682,#15683,#15684,
#15685,#15686,#15687,#15688,#15689,#15690,#15691,#15692,#15693,#15694,#15695,
#15696,#15697,#15698,#15699,#15700,#15701),.UNSPECIFIED.,.F.,.F.,(4,3,3,
3,3,3,3,4),(20.1591190625158,20.9674586918964,21.9659091057962,22.9643595196961,
23.9628099335959,24.9612603474957,25.9597107613956,26.4423043696954),
 .UNSPECIFIED.);
#1818=B_SPLINE_CURVE_WITH_KNOTS('',3,(#15702,#15703,#15704,#15705,#15706,
#15707,#15708,#15709,#15710,#15711,#15712,#15713,#15714,#15715,#15716,#15717,
#15718,#15719,#15720,#15721,#15722,#15723),.UNSPECIFIED.,.F.,.F.,(4,3,3,
3,3,3,3,4),(-22.6985303271799,-21.9659091057962,-20.9674586918964,-19.9690082779966,
-18.9705578640968,-17.9721074501969,-16.9736570362971,-16.4153450200003),
 .UNSPECIFIED.);
#1819=B_SPLINE_CURVE_WITH_KNOTS('',3,(#15728,#15729,#15730,#15731,#15732,
#15733,#15734,#15735,#15736,#15737,#15738,#15739,#15740,#15741,#15742,#15743,
#15744,#15745,#15746,#15747,#15748,#15749,#15750,#15751,#15752),
 .UNSPECIFIED.,.F.,.F.,(4,3,3,3,3,3,3,3,4),(13.8759337553362,13.9783057945976,
14.9767562084974,15.9752066223973,16.9736570362971,17.9721074501969,18.9705578640968,
19.9690082779966,20.1591190625158),.UNSPECIFIED.);
#1820=B_SPLINE_CURVE_WITH_KNOTS('',3,(#15753,#15754,#15755,#15756,#15757,
#15758,#15759,#15760,#15761,#15762,#15763,#15764,#15765,#15766,#15767,#15768,
#15769,#15770,#15771,#15772,#15773,#15774),.UNSPECIFIED.,.F.,.F.,(4,3,3,
3,3,3,3,4),(-16.4153450200003,-15.9752066223973,-14.9767562084974,-13.9783057945976,
-12.9798553806978,-11.9814049667979,-10.9829545528981,-10.1321597128207),
 .UNSPECIFIED.);
#1821=B_SPLINE_CURVE_WITH_KNOTS('',3,(#15780,#15781,#15782,#15783,#15784,
#15785,#15786,#15787,#15788,#15789,#15790,#15791,#15792),.UNSPECIFIED.,
 .F.,.F.,(4,3,3,3,4),(-3.84897440564114,-2.99535124169948,-1.99690082779965,
-0.99845041389982,0.),.UNSPECIFIED.);
#1822=B_SPLINE_CURVE_WITH_KNOTS('',3,(#15795,#15796,#15797,#15798,#15799,
#15800,#15801,#15802,#15803,#15804,#15805,#15806,#15807,#15808,#15809,#15810,
#15811,#15812,#15813),.UNSPECIFIED.,.F.,.F.,(4,3,3,3,3,3,4),(2.01694489302848,
2.99535124169948,3.99380165559931,4.99225206949914,5.99070248339897,6.9891528972988,
7.59274844815661),.UNSPECIFIED.);
#1823=B_SPLINE_CURVE_WITH_KNOTS('',3,(#15819,#15820,#15821,#15822,#15823,
#15824,#15825,#15826),.UNSPECIFIED.,.F.,.F.,(4,1,1,1,1,4),(116.238928182822,
116.69628232179,117.69473273569,118.693183149589,119.691633563489,120.690083977389),
 .UNSPECIFIED.);
#1824=B_SPLINE_CURVE_WITH_KNOTS('',3,(#15829,#15830,#15831,#15832,#15833,
#15834,#15835,#15836,#15837),.UNSPECIFIED.,.F.,.F.,(4,1,1,1,1,1,4),(116.238928182822,
116.240342344754,117.238792758654,118.237243172554,119.235693586454,120.234144000354,
121.212550349025),.UNSPECIFIED.);
#1825=B_SPLINE_CURVE_WITH_KNOTS('',3,(#15842,#15843,#15844,#15845,#15846,
#15847,#15848,#15849,#15850,#15851),.UNSPECIFIED.,.F.,.F.,(4,1,1,1,1,1,
1,4),(109.955742875643,110.705579838391,111.704030252291,112.70248066619,
113.70093108009,114.69938149399,115.69783190789,116.238928182822),
 .UNSPECIFIED.);
#1826=B_SPLINE_CURVE_WITH_KNOTS('',3,(#15852,#15853,#15854,#15855,#15856,
#15857,#15858,#15859,#15860,#15861),.UNSPECIFIED.,.F.,.F.,(4,1,1,1,1,1,
1,4),(109.955742875643,110.249639861355,111.248090275255,112.246540689155,
113.244991103055,114.243441516955,115.241891930855,116.238928182822),
 .UNSPECIFIED.);
#1827=B_SPLINE_CURVE_WITH_KNOTS('',3,(#15866,#15867,#15868,#15869,#15870,
#15871,#15872,#15873,#15874,#15875,#15876),.UNSPECIFIED.,.F.,.F.,(4,1,1,
1,1,1,1,1,4),(103.672557568463,103.716426941092,104.714877354992,105.713327768892,
106.711778182792,107.710228596691,108.708679010591,109.707129424491,109.955742875643),
 .UNSPECIFIED.);
#1828=B_SPLINE_CURVE_WITH_KNOTS('',3,(#15877,#15878,#15879,#15880,#15881,
#15882,#15883,#15884,#15885,#15886),.UNSPECIFIED.,.F.,.F.,(4,1,1,1,1,1,
1,4),(103.672557568463,104.258937377956,105.257387791856,106.255838205756,
107.254288619656,108.252739033556,109.251189447456,109.955742875643),
 .UNSPECIFIED.);
#1829=B_SPLINE_CURVE_WITH_KNOTS('',3,(#15891,#15892,#15893,#15894,#15895,
#15896,#15897,#15898,#15899,#15900),.UNSPECIFIED.,.F.,.F.,(4,1,1,1,1,1,
1,4),(97.3893722612835,97.7257244576931,98.7241748715929,99.7226252854927,
100.721075699393,101.719526113292,102.717976527192,103.672557568463),
 .UNSPECIFIED.);
#1830=B_SPLINE_CURVE_WITH_KNOTS('',3,(#15901,#15902,#15903,#15904,#15905,
#15906,#15907,#15908,#15909,#15910),.UNSPECIFIED.,.F.,.F.,(4,1,1,1,1,1,
1,4),(97.3893722612835,98.2682348945574,99.2666853084573,100.265135722357,
101.263586136257,102.262036550157,103.260486964057,103.672557568463),
 .UNSPECIFIED.);
#1831=B_SPLINE_CURVE_WITH_KNOTS('',3,(#15915,#15916,#15917,#15918,#15919,
#15920,#15921,#15922,#15923,#15924),.UNSPECIFIED.,.F.,.F.,(4,1,1,1,1,1,
1,4),(91.106186954104,91.7350219742941,92.7334723881939,93.7319228020937,
94.7303732159936,95.7288236298934,96.7272740437932,97.3893722612835),
 .UNSPECIFIED.);
#1832=B_SPLINE_CURVE_WITH_KNOTS('',3,(#15925,#15926,#15927,#15928,#15929,
#15930,#15931,#15932,#15933,#15934,#15935),.UNSPECIFIED.,.F.,.F.,(4,1,1,
1,1,1,1,1,4),(91.106186954104,91.2790819972586,92.2775324111584,93.2759828250583,
94.2744332389581,95.2728836528579,96.2713340667578,97.2697844806576,97.3893722612835),
 .UNSPECIFIED.);
#1833=B_SPLINE_CURVE_WITH_KNOTS('',3,(#15940,#15941,#15942,#15943,#15944,
#15945,#15946,#15947,#15948,#15949),.UNSPECIFIED.,.F.,.F.,(4,1,1,1,1,1,
1,4),(84.8230016469244,85.7443194908951,86.7427699047949,87.7412203186948,
88.7396707325946,89.7381211464944,90.7365715603943,91.106186954104),
 .UNSPECIFIED.);
#1834=B_SPLINE_CURVE_WITH_KNOTS('',3,(#15950,#15951,#15952,#15953,#15954,
#15955,#15956,#15957,#15958,#15959),.UNSPECIFIED.,.F.,.F.,(4,1,1,1,1,1,
1,4),(84.8230016469244,85.2883795138596,86.2868299277595,87.2852803416593,
88.2837307555591,89.282181169459,90.2806315833588,91.106186954104),
 .UNSPECIFIED.);
#1835=B_SPLINE_CURVE_WITH_KNOTS('',3,(#15964,#15965,#15966,#15967,#15968,
#15969,#15970,#15971,#15972,#15973,#15974),.UNSPECIFIED.,.F.,.F.,(4,1,1,
1,1,1,1,1,4),(78.5398163397448,78.7551665935963,79.7536170074961,80.7520674213959,
81.7505178352958,82.7489682491956,83.7474186630954,84.7458690769953,84.8230016469244),
 .UNSPECIFIED.);
#1836=B_SPLINE_CURVE_WITH_KNOTS('',3,(#15975,#15976,#15977,#15978,#15979,
#15980,#15981,#15982,#15983,#15984),.UNSPECIFIED.,.F.,.F.,(4,1,1,1,1,1,
1,4),(78.5398163397448,79.2976770304607,80.2961274443605,81.2945778582603,
82.2930282721602,83.29147868606,84.2899290999598,84.8230016469244),
 .UNSPECIFIED.);
#1837=B_SPLINE_CURVE_WITH_KNOTS('',3,(#15989,#15990,#15991,#15992,#15993,
#15994,#15995,#15996,#15997,#15998),.UNSPECIFIED.,.F.,.F.,(4,1,1,1,1,1,
1,4),(72.2566310325652,72.7644641101973,73.7629145240972,74.761364937997,
75.7598153518968,76.7582657657966,77.7567161796965,78.5398163397448),
 .UNSPECIFIED.);
#1838=B_SPLINE_CURVE_WITH_KNOTS('',3,(#15999,#16000,#16001,#16002,#16003,
#16004,#16005,#16006,#16007,#16008,#16009),.UNSPECIFIED.,.F.,.F.,(4,1,1,
1,1,1,1,1,4),(72.2566310325652,72.3085241331619,73.3069745470617,74.3054249609615,
75.3038753748613,76.3023257887612,77.300776202661,78.2992266165608,78.5398163397448),
 .UNSPECIFIED.);
#1839=B_SPLINE_CURVE_WITH_KNOTS('',3,(#16014,#16015,#16016,#16017,#16018,
#16019,#16020,#16021,#16022,#16023),.UNSPECIFIED.,.F.,.F.,(4,1,1,1,1,1,
1,4),(65.9734457253856,66.7737616267983,67.7722120406982,68.770662454598,
69.7691128684978,70.7675632823977,71.7660136962975,72.2566310325652),
 .UNSPECIFIED.);
#1840=B_SPLINE_CURVE_WITH_KNOTS('',3,(#16024,#16025,#16026,#16027,#16028,
#16029,#16030,#16031,#16032,#16033),.UNSPECIFIED.,.F.,.F.,(4,1,1,1,1,1,
1,4),(65.9734457253856,66.3178216497629,67.3162720636627,68.3147224775625,
69.3131728914624,70.3116233053622,71.310073719262,72.2566310325652),
 .UNSPECIFIED.);
#1841=B_SPLINE_CURVE_WITH_KNOTS('',3,(#16038,#16039,#16040,#16041,#16042,
#16043,#16044,#16045,#16046,#16047,#16048),.UNSPECIFIED.,.F.,.F.,(4,1,1,
1,1,1,1,1,4),(59.690260418206,59.7846087294995,60.7830591433994,61.7815095572992,
62.779959971199,63.7784103850989,64.7768607989987,65.7753112128985,65.9734457253856),
 .UNSPECIFIED.);
#1842=B_SPLINE_CURVE_WITH_KNOTS('',3,(#16049,#16050,#16051,#16052,#16053,
#16054,#16055,#16056,#16057,#16058),.UNSPECIFIED.,.F.,.F.,(4,1,1,1,1,1,
1,4),(59.690260418206,60.3271191663639,61.3255695802637,62.3240199941636,
63.3224704080634,64.3209208219632,65.3193712358631,65.9734457253856),
 .UNSPECIFIED.);
#1843=B_SPLINE_CURVE_WITH_KNOTS('',3,(#16063,#16064,#16065,#16066,#16067,
#16068,#16069,#16070,#16071,#16072),.UNSPECIFIED.,.F.,.F.,(4,1,1,1,1,1,
1,4),(53.4070751110264,53.7939062461006,54.7923566600004,55.7908070739002,
56.7892574878001,57.7877079016999,58.7861583155997,59.690260418206),
 .UNSPECIFIED.);
#1844=B_SPLINE_CURVE_WITH_KNOTS('',3,(#16073,#16074,#16075,#16076,#16077,
#16078,#16079,#16080,#16081,#16082),.UNSPECIFIED.,.F.,.F.,(4,1,1,1,1,1,
1,4),(53.4070751110264,54.3364166829649,55.3348670968648,56.3333175107646,
57.3317679246644,58.3302183385643,59.3286687524641,59.690260418206),
 .UNSPECIFIED.);
#1845=B_SPLINE_CURVE_WITH_KNOTS('',3,(#16087,#16088,#16089,#16090,#16091,
#16092,#16093,#16094,#16095,#16096),.UNSPECIFIED.,.F.,.F.,(4,1,1,1,1,1,
1,4),(47.1238898038468,47.8032037627016,48.8016541766014,49.8001045905012,
50.7985550044011,51.7970054183009,52.7954558322007,53.4070751110264),
 .UNSPECIFIED.);
#1846=B_SPLINE_CURVE_WITH_KNOTS('',3,(#16097,#16098,#16099,#16100,#16101,
#16102,#16103,#16104,#16105,#16106,#16107),.UNSPECIFIED.,.F.,.F.,(4,1,1,
1,1,1,1,1,4),(47.1238898038468,47.3472637856661,48.345714199566,49.3441646134658,
50.3426150273656,51.3410654412654,52.3395158551653,53.3379662690651,53.4070751110264),
 .UNSPECIFIED.);
#1847=B_SPLINE_CURVE_WITH_KNOTS('',3,(#16112,#16113,#16114,#16115,#16116,
#16117,#16118,#16119,#16120,#16121),.UNSPECIFIED.,.F.,.F.,(4,1,1,1,1,1,
1,4),(40.8407044966672,41.8125012793026,42.8109516932024,43.8094021071023,
44.8078525210021,45.8063029349019,46.8047533488018,47.1238898038468),
 .UNSPECIFIED.);
#1848=B_SPLINE_CURVE_WITH_KNOTS('',3,(#16122,#16123,#16124,#16125,#16126,
#16127,#16128,#16129,#16130,#16131),.UNSPECIFIED.,.F.,.F.,(4,1,1,1,1,1,
1,4),(40.8407044966672,41.3565613022672,42.355011716167,43.3534621300668,
44.3519125439666,45.3503629578665,46.3488133717663,47.1238898038468),
 .UNSPECIFIED.);
#1849=B_SPLINE_CURVE_WITH_KNOTS('',3,(#16136,#16137,#16138,#16139,#16140,
#16141,#16142,#16143,#16144,#16145,#16146),.UNSPECIFIED.,.F.,.F.,(4,1,1,
1,1,1,1,1,4),(34.5575191894876,34.8233483820038,35.8217987959036,36.8202492098035,
37.8186996237033,38.8171500376031,39.8156004515029,40.8140508654028,40.8407044966672),
 .UNSPECIFIED.);
#1850=B_SPLINE_CURVE_WITH_KNOTS('',3,(#16147,#16148,#16149,#16150,#16151,
#16152,#16153,#16154,#16155,#16156),.UNSPECIFIED.,.F.,.F.,(4,1,1,1,1,1,
1,4),(34.5575191894876,35.3658588188682,36.364309232768,37.3627596466678,
38.3612100605677,39.3596604744675,40.3581108883673,40.8407044966672),
 .UNSPECIFIED.);
#1851=B_SPLINE_CURVE_WITH_KNOTS('',3,(#16161,#16162,#16163,#16164,#16165,
#16166,#16167,#16168,#16169,#16170),.UNSPECIFIED.,.F.,.F.,(4,1,1,1,1,1,
1,4),(28.274333882308,28.8326458986048,29.8310963125046,30.8295467264045,
31.8279971403043,32.8264475542041,33.824897968104,34.5575191894876),
 .UNSPECIFIED.);
#1852=B_SPLINE_CURVE_WITH_KNOTS('',3,(#16171,#16172,#16173,#16174,#16175,
#16176,#16177,#16178,#16179,#16180,#16181),.UNSPECIFIED.,.F.,.F.,(4,1,1,
1,1,1,1,1,4),(28.274333882308,28.3767059215694,29.3751563354692,30.373606749369,
31.3720571632689,32.3705075771687,33.3689579910685,34.3674084049683,34.5575191894876),
 .UNSPECIFIED.);
#1853=B_SPLINE_CURVE_WITH_KNOTS('',3,(#16186,#16187,#16188,#16189,#16190,
#16191,#16192,#16193,#16194,#16195),.UNSPECIFIED.,.F.,.F.,(4,1,1,1,1,1,
1,4),(21.9911485751285,22.8419434152058,23.8403938291057,24.8388442430055,
25.8372946569053,26.8357450708052,27.834195484705,28.274333882308),
 .UNSPECIFIED.);
#1854=B_SPLINE_CURVE_WITH_KNOTS('',3,(#16196,#16197,#16198,#16199,#16200,
#16201,#16202,#16203,#16204,#16205),.UNSPECIFIED.,.F.,.F.,(4,1,1,1,1,1,
1,4),(21.9911485751284,22.3860034381704,23.3844538520702,24.3829042659701,
25.3813546798699,26.3798050937697,27.3782555076695,28.274333882308),
 .UNSPECIFIED.);
#1855=B_SPLINE_CURVE_WITH_KNOTS('',3,(#16211,#16212,#16213,#16214,#16215),
 .UNSPECIFIED.,.F.,.F.,(4,1,4),(14.3984001269718,15.3968505408716,15.7079632679489),
 .UNSPECIFIED.);
#1856=B_SPLINE_CURVE_WITH_KNOTS('',3,(#16218,#16219,#16220,#16221,#16222),
 .UNSPECIFIED.,.F.,.F.,(4,1,4),(13.8759337553362,14.8543401040072,15.7079632679489),
 .UNSPECIFIED.);
#1857=B_SPLINE_CURVE_WITH_KNOTS('',3,(#16224,#16225,#16226,#16227,#16228,
#16229,#16230,#16231,#16232,#16233,#16234,#16235,#16236,#16237,#16238,#16239,
#16240,#16241,#16242,#16243,#16244,#16245,#16246,#16247,#16248,#16249,#16250,
#16251,#16252,#16253,#16254,#16255,#16256,#16257,#16258,#16259,#16260,#16261,
#16262,#16263,#16264,#16265,#16266,#16267,#16268,#16269,#16270,#16271,#16272,
#16273,#16274,#16275,#16276,#16277,#16278,#16279,#16280,#16281,#16282,#16283,
#16284,#16285,#16286,#16287,#16288,#16289,#16290,#16291,#16292,#16293,#16294,
#16295,#16296,#16297,#16298,#16299,#16300,#16301,#16302,#16303,#16304,#16305,
#16306,#16307,#16308,#16309,#16310,#16311,#16312,#16313,#16314),
 .UNSPECIFIED.,.F.,.F.,(4,3,3,3,3,3,3,3,3,3,3,3,3,3,3,3,3,3,3,3,3,3,3,3,
3,3,3,3,3,3,4),(-0.569248610399407,-0.543578596463163,-0.517279330488097,
-0.510427274183678,-0.504800560895351,-0.477739172209543,-0.455689330734177,
-0.448366213390789,-0.442461660719966,-0.41472996294248,-0.386382582308514,
-0.358441367058857,-0.343970572338644,-0.337413249439412,-0.308477582949163,
-0.301340440406615,-0.273499497437324,-0.245035895034271,-0.233720105006401,
-0.228077781576704,-0.199099310593537,-0.169543243081912,-0.139741771809077,
-0.123046919548663,-0.118260996555259,-0.114011653396177,-0.08346298006925,
-0.0528795458366397,-0.0229338899610989,-0.00618295372576638,0.),
 .UNSPECIFIED.);
#1858=B_SPLINE_CURVE_WITH_KNOTS('',3,(#16315,#16316,#16317,#16318,#16319,
#16320,#16321,#16322,#16323,#16324,#16325,#16326,#16327,#16328,#16329,#16330,
#16331,#16332,#16333,#16334,#16335,#16336,#16337,#16338,#16339,#16340,#16341,
#16342,#16343,#16344,#16345,#16346,#16347,#16348,#16349,#16350,#16351,#16352,
#16353,#16354,#16355,#16356,#16357,#16358,#16359,#16360,#16361,#16362,#16363,
#16364,#16365,#16366,#16367,#16368,#16369,#16370,#16371,#16372,#16373,#16374,
#16375,#16376,#16377,#16378,#16379,#16380,#16381,#16382,#16383,#16384,#16385,
#16386,#16387,#16388,#16389,#16390,#16391,#16392,#16393,#16394,#16395,#16396,
#16397,#16398,#16399,#16400,#16401,#16402,#16403,#16404,#16405),
 .UNSPECIFIED.,.F.,.F.,(4,3,3,3,3,3,3,3,3,3,3,3,3,3,3,3,3,3,3,3,3,3,3,3,
3,3,3,3,3,3,4),(-0.566847306048068,-0.536667790777227,-0.506059605580284,
-0.497462088050579,-0.490486593578347,-0.460335737779737,-0.436884523306703,
-0.424130100459425,-0.418922747352239,-0.389496677338306,-0.360304013502597,
-0.332014662955751,-0.317192502715681,-0.312071570778799,-0.307326824244741,
-0.279357757008042,-0.27272602199547,-0.244230768419255,-0.21433741748379,
-0.205052770738313,-0.200811095462912,-0.172975232517528,-0.145198207857396,
-0.117889770880004,-0.103789044636945,-0.0993778831760535,-0.0726518756869364,
-0.0463552868969829,-0.0209007422778119,-0.00508396093552814,0.),
 .UNSPECIFIED.);
#1859=B_SPLINE_CURVE_WITH_KNOTS('',3,(#16407,#16408,#16409,#16410,#16411,
#16412,#16413,#16414,#16415,#16416,#16417),.UNSPECIFIED.,.F.,.F.,(4,1,1,
1,1,1,1,1,4),(15.7079632679489,15.852790517907,16.8512409318069,17.8496913457067,
18.8481417596065,19.8465921735064,20.8450425874062,21.843493001306,21.9911485751285),
 .UNSPECIFIED.);
#1860=B_SPLINE_CURVE_WITH_KNOTS('',3,(#16418,#16419,#16420,#16421,#16422,
#16423,#16424,#16425,#16426,#16427),.UNSPECIFIED.,.F.,.F.,(4,1,1,1,1,1,
1,4),(15.7079632679489,16.3953009547714,17.3937513686712,18.3922017825711,
19.3906521964709,20.3891026103707,21.3875530242706,21.9911485751284),
 .UNSPECIFIED.);
#1861=B_SPLINE_CURVE_WITH_KNOTS('',3,(#16876,#16877,#16878,#16879,#16880,
#16881,#16882,#16883,#16884,#16885,#16886,#16887,#16888,#16889,#16890,#16891,
#16892,#16893,#16894,#16895,#16896,#16897,#16898,#16899,#16900,#16901,#16902,
#16903,#16904,#16905,#16906,#16907,#16908,#16909,#16910,#16911,#16912,#16913,
#16914,#16915,#16916,#16917,#16918,#16919,#16920,#16921,#16922,#16923,#16924,
#16925,#16926,#16927,#16928,#16929,#16930,#16931,#16932,#16933,#16934,#16935,
#16936,#16937,#16938,#16939,#16940,#16941,#16942,#16943,#16944,#16945,#16946,
#16947,#16948,#16949,#16950,#16951,#16952,#16953,#16954,#16955,#16956,#16957,
#16958,#16959,#16960,#16961,#16962,#16963,#16964,#16965,#16966,#16967,#16968,
#16969,#16970,#16971,#16972),.UNSPECIFIED.,.F.,.F.,(4,3,3,3,3,3,3,3,3,3,
3,3,3,3,3,3,3,3,3,3,3,3,3,3,3,3,3,3,3,3,3,3,4),(0.,0.0253589562758107,0.0513899835108827,
0.0783515483041457,0.0901472329011983,0.0965516813294443,0.102699177545927,
0.130000868916647,0.157755246288974,0.185087060180977,0.195806070593553,
0.20210936686077,0.206420439750695,0.235022976376574,0.26352929739743,0.267082501856987,
0.294994868256452,0.306190141773776,0.311401074814444,0.315730762045215,
0.3438256131073,0.372960412553192,0.402414247073163,0.414012338023885,0.420579327404534,
0.426866604939584,0.456917898655282,0.482860587387028,0.492968514404809,
0.498516388426713,0.52960252100449,0.560688653582267,0.566847306048208),
 .UNSPECIFIED.);
#1862=B_SPLINE_CURVE_WITH_KNOTS('',3,(#16973,#16974,#16975,#16976,#16977,
#16978,#16979,#16980,#16981,#16982,#16983,#16984,#16985,#16986,#16987,#16988,
#16989,#16990,#16991,#16992,#16993,#16994,#16995,#16996,#16997),
 .UNSPECIFIED.,.F.,.F.,(4,3,3,3,3,3,3,3,4),(-10.1321597128207,-9.98450413899829,
-8.98605372509846,-7.98760331119862,-6.9891528972988,-5.99070248339897,
-4.99225206949914,-3.99380165559931,-3.84897440564114),.UNSPECIFIED.);
#1863=B_SPLINE_CURVE_WITH_KNOTS('',3,(#17446,#17447,#17448,#17449,#17450,
#17451,#17452,#17453,#17454,#17455,#17456,#17457,#17458,#17459,#17460,#17461,
#17462,#17463,#17464,#17465,#17466,#17467),.UNSPECIFIED.,.F.,.F.,(4,3,3,
3,3,3,3,4),(7.59274844815661,7.98760331119863,8.98605372509846,9.98450413899829,
10.9829545528981,11.981404966798,12.9798553806978,13.8759337553362),
 .UNSPECIFIED.);
#1864=B_SPLINE_CURVE_WITH_KNOTS('',3,(#17468,#17469,#17470,#17471,#17472,
#17473,#17474,#17475,#17476,#17477,#17478,#17479,#17480,#17481,#17482,#17483,
#17484,#17485,#17486,#17487,#17488,#17489,#17490,#17491,#17492,#17493,#17494,
#17495,#17496,#17497,#17498,#17499,#17500,#17501,#17502,#17503,#17504,#17505,
#17506,#17507,#17508,#17509,#17510,#17511,#17512,#17513,#17514,#17515,#17516,
#17517,#17518,#17519,#17520,#17521,#17522,#17523,#17524,#17525,#17526,#17527,
#17528,#17529,#17530,#17531,#17532,#17533,#17534,#17535,#17536,#17537,#17538,
#17539,#17540,#17541,#17542,#17543,#17544,#17545,#17546,#17547,#17548,#17549,
#17550,#17551,#17552,#17553,#17554,#17555,#17556,#17557,#17558,#17559,#17560,
#17561),.UNSPECIFIED.,.F.,.F.,(4,3,3,3,3,3,3,3,3,3,3,3,3,3,3,3,3,3,3,3,
3,3,3,3,3,3,3,3,3,3,3,4),(0.,0.0297203831394795,0.0601035467162832,0.0895497219052599,
0.115315125195615,0.120671839320256,0.150435254338286,0.180035115203003,
0.208944573459276,0.221427488552219,0.230458159732982,0.23471220724889,
0.263249756710517,0.291154363988279,0.295672948228097,0.324625445746226,
0.334643738865253,0.339478705934468,0.343237386322571,0.371326757387601,
0.39947478984986,0.427227777476084,0.438024540249258,0.443793094729609,
0.448942971696371,0.476234898938785,0.49821292729788,0.507328693746962,
0.512107928640037,0.538127470507601,0.564147012375166,0.569248610399473),
 .UNSPECIFIED.);
#1865=B_SPLINE_CURVE_WITH_KNOTS('',3,(#17564,#17565,#17566,#17567,#17568,
#17569,#17570,#17571,#17572,#17573,#17574,#17575,#17576,#17577,#17578,#17579,
#17580,#17581,#17582,#17583,#17584,#17585,#17586,#17587,#17588,#17589,#17590,
#17591,#17592,#17593,#17594,#17595,#17596,#17597,#17598,#17599,#17600,#17601,
#17602,#17603,#17604,#17605,#17606,#17607,#17608,#17609,#17610,#17611,#17612,
#17613,#17614,#17615,#17616,#17617,#17618,#17619,#17620,#17621,#17622,#17623,
#17624,#17625,#17626,#17627,#17628,#17629,#17630,#17631,#17632,#17633,#17634,
#17635,#17636,#17637,#17638,#17639,#17640,#17641,#17642,#17643,#17644,#17645,
#17646,#17647,#17648,#17649,#17650,#17651,#17652,#17653,#17654),
 .UNSPECIFIED.,.F.,.F.,(4,3,3,3,3,3,3,3,3,3,3,3,3,3,3,3,3,3,3,3,3,3,3,3,
3,3,3,3,3,3,4),(-0.569248610399443,-0.543578588652014,-0.517279316104031,
-0.510427238217388,-0.504800560499363,-0.477739166329021,-0.45568932558873,
-0.448366156831823,-0.442461645413569,-0.41472994217853,-0.386382566735571,
-0.358441354206424,-0.343970553035952,-0.337413258055178,-0.308477591793723,
-0.301340440406694,-0.273499502259986,-0.245035902856791,-0.233720101852398,
-0.228077781614374,-0.199099314524288,-0.169543248975156,-0.139741777996353,
-0.123046924962531,-0.11826102155782,-0.11401170878925,-0.083463036592537,
-0.0528796019523826,-0.0229339459431555,-0.0061829537257795,0.),
 .UNSPECIFIED.);
#1866=B_SPLINE_CURVE_WITH_KNOTS('',3,(#17655,#17656,#17657,#17658,#17659,
#17660,#17661,#17662,#17663,#17664,#17665,#17666,#17667,#17668,#17669,#17670,
#17671,#17672,#17673,#17674,#17675,#17676,#17677,#17678,#17679,#17680,#17681,
#17682,#17683,#17684,#17685,#17686,#17687,#17688,#17689,#17690,#17691,#17692,
#17693,#17694,#17695,#17696,#17697,#17698,#17699,#17700,#17701,#17702,#17703,
#17704,#17705,#17706,#17707,#17708,#17709,#17710,#17711,#17712,#17713,#17714,
#17715,#17716,#17717,#17718,#17719,#17720,#17721,#17722,#17723,#17724,#17725,
#17726,#17727,#17728,#17729,#17730,#17731,#17732,#17733,#17734,#17735,#17736,
#17737,#17738,#17739,#17740,#17741,#17742,#17743,#17744,#17745),
 .UNSPECIFIED.,.F.,.F.,(4,3,3,3,3,3,3,3,3,3,3,3,3,3,3,3,3,3,3,3,3,3,3,3,
3,3,3,3,3,3,4),(-0.566847306048142,-0.536667785913132,-0.50605959936329,
-0.497462080219576,-0.490486592168179,-0.460335736468636,-0.436884522159495,
-0.424130097594776,-0.418922746580067,-0.38949667718092,-0.360304013384567,
-0.332014664357047,-0.317192503766662,-0.312071575644096,-0.307326824831242,
-0.279357759469794,-0.272726021995507,-0.244230768475208,-0.214337417532747,
-0.20505277122677,-0.200811095853765,-0.172975232543609,-0.145198207986257,
-0.117889772593011,-0.103789046135826,-0.0993778841074578,-0.0726518774649773,
-0.0463552908642349,-0.020900750299918,-0.00508396093552477,0.),
 .UNSPECIFIED.);
#1867=B_SPLINE_CURVE_WITH_KNOTS('',3,(#17747,#17748,#17749,#17750,#17751,
#17752,#17753,#17754,#17755,#17756,#17757),.UNSPECIFIED.,.F.,.F.,(4,1,1,
1,1,1,1,1,4),(15.7079632679489,15.852790517907,16.8512409318069,17.8496913457067,
18.8481417596065,19.8465921735064,20.8450425874062,21.843493001306,21.9911485751285),
 .UNSPECIFIED.);
#1868=B_SPLINE_CURVE_WITH_KNOTS('',3,(#17758,#17759,#17760,#17761,#17762,
#17763,#17764,#17765,#17766,#17767),.UNSPECIFIED.,.F.,.F.,(4,1,1,1,1,1,
1,4),(15.7079632679489,16.3953009547714,17.3937513686712,18.3922017825711,
19.3906521964709,20.3891026103707,21.3875530242706,21.9911485751284),
 .UNSPECIFIED.);
#1869=B_SPLINE_CURVE_WITH_KNOTS('',3,(#18216,#18217,#18218,#18219,#18220,
#18221,#18222,#18223,#18224,#18225,#18226,#18227,#18228,#18229,#18230,#18231,
#18232,#18233,#18234,#18235,#18236,#18237,#18238,#18239,#18240,#18241,#18242,
#18243,#18244,#18245,#18246,#18247,#18248,#18249,#18250,#18251,#18252,#18253,
#18254,#18255,#18256,#18257,#18258,#18259,#18260,#18261,#18262,#18263,#18264,
#18265,#18266,#18267,#18268,#18269,#18270,#18271,#18272,#18273,#18274,#18275,
#18276,#18277,#18278,#18279,#18280,#18281,#18282,#18283,#18284,#18285,#18286,
#18287,#18288,#18289,#18290,#18291,#18292,#18293,#18294,#18295,#18296,#18297,
#18298,#18299,#18300,#18301,#18302,#18303,#18304,#18305,#18306,#18307,#18308,
#18309,#18310,#18311,#18312),.UNSPECIFIED.,.F.,.F.,(4,3,3,3,3,3,3,3,3,3,
3,3,3,3,3,3,3,3,3,3,3,3,3,3,3,3,3,3,3,3,3,3,4),(0.,0.0253589640191775,0.0513899982793661,
0.0783515612265618,0.0901472450159599,0.0965516873007117,0.102699175683727,
0.130000872479608,0.157755252595204,0.185087064910636,0.195806071974665,
0.202109368589621,0.206420440483056,0.235022978557914,0.263529297383441,
0.267082501856932,0.294994864743443,0.306190136087185,0.311401050641315,
0.315730756609606,0.343825602488203,0.372960399516403,0.402414233419896,
0.414012310566607,0.42057914219519,0.426866594758845,0.456917887218389,
0.48286057880933,0.492968489082692,0.498516363071224,0.529602508326689,
0.560688653582154,0.566847306048091),.UNSPECIFIED.);
#1870=B_SPLINE_CURVE_WITH_KNOTS('',3,(#18313,#18314,#18315,#18316,#18317,
#18318,#18319,#18320,#18321,#18322,#18323,#18324,#18325,#18326,#18327,#18328,
#18329,#18330,#18331,#18332,#18333,#18334,#18335,#18336,#18337),
 .UNSPECIFIED.,.F.,.F.,(4,3,3,3,3,3,3,3,4),(-10.1321597128207,-9.98450413899829,
-8.98605372509846,-7.98760331119863,-6.9891528972988,-5.99070248339897,
-4.99225206949914,-3.99380165559932,-3.84897440564114),.UNSPECIFIED.);
#1871=B_SPLINE_CURVE_WITH_KNOTS('',3,(#18786,#18787,#18788,#18789,#18790,
#18791,#18792,#18793,#18794,#18795,#18796,#18797,#18798,#18799,#18800,#18801,
#18802,#18803,#18804,#18805,#18806,#18807),.UNSPECIFIED.,.F.,.F.,(4,3,3,
3,3,3,3,4),(7.59274844815663,7.98760331119864,8.98605372509847,9.9845041389983,
10.9829545528981,11.981404966798,12.9798553806978,13.8759337553362),
 .UNSPECIFIED.);
#1872=B_SPLINE_CURVE_WITH_KNOTS('',3,(#18808,#18809,#18810,#18811,#18812,
#18813,#18814,#18815,#18816,#18817,#18818,#18819,#18820,#18821,#18822,#18823,
#18824,#18825,#18826,#18827,#18828,#18829,#18830,#18831,#18832,#18833,#18834,
#18835,#18836,#18837,#18838,#18839,#18840,#18841,#18842,#18843,#18844,#18845,
#18846,#18847,#18848,#18849,#18850,#18851,#18852,#18853,#18854,#18855,#18856,
#18857,#18858,#18859,#18860,#18861,#18862,#18863,#18864,#18865,#18866,#18867,
#18868,#18869,#18870,#18871,#18872,#18873,#18874,#18875,#18876,#18877,#18878,
#18879,#18880,#18881,#18882,#18883,#18884,#18885,#18886,#18887,#18888,#18889,
#18890,#18891,#18892,#18893,#18894,#18895,#18896,#18897,#18898,#18899,#18900,
#18901),.UNSPECIFIED.,.F.,.F.,(4,3,3,3,3,3,3,3,3,3,3,3,3,3,3,3,3,3,3,3,
3,3,3,3,3,3,3,3,3,3,3,4),(0.,0.0297203899945205,0.06010355702558,0.0895497309258828,
0.115315133088648,0.120671841145989,0.150435256327594,0.180035115425351,
0.208944573626014,0.221427487940053,0.230458155185264,0.234712201077947,
0.263249748593671,0.291154354340093,0.295672948228002,0.324625446145178,
0.334643737982065,0.339478702992735,0.343237383195306,0.371326754477909,
0.399474787132745,0.427227773598525,0.438024531377961,0.443793087224999,
0.448942972295281,0.476234898815801,0.498212927205595,0.507328692507987,
0.512107925785297,0.538127469080138,0.564147012374979,0.569248610399289),
 .UNSPECIFIED.);
#1873=B_SPLINE_CURVE_WITH_KNOTS('',3,(#18904,#18905,#18906,#18907,#18908,
#18909,#18910,#18911,#18912,#18913,#18914,#18915,#18916,#18917,#18918,#18919,
#18920,#18921,#18922,#18923,#18924,#18925,#18926,#18927,#18928,#18929,#18930,
#18931,#18932,#18933,#18934,#18935,#18936,#18937,#18938,#18939,#18940,#18941,
#18942,#18943,#18944,#18945,#18946,#18947,#18948,#18949,#18950,#18951,#18952,
#18953,#18954,#18955,#18956,#18957,#18958,#18959,#18960,#18961,#18962,#18963,
#18964,#18965,#18966,#18967,#18968,#18969,#18970,#18971,#18972,#18973,#18974,
#18975,#18976,#18977,#18978,#18979,#18980,#18981,#18982,#18983,#18984,#18985,
#18986,#18987,#18988,#18989,#18990,#18991,#18992,#18993,#18994),
 .UNSPECIFIED.,.F.,.F.,(4,3,3,3,3,3,3,3,3,3,3,3,3,3,3,3,3,3,3,3,3,3,3,3,
3,3,3,3,3,3,4),(-0.569248610399526,-0.543579431798118,-0.517280869422508,
-0.510431120482963,-0.504800591464605,-0.47773979012753,-0.455689871412427,
-0.448372136428178,-0.442463258694081,-0.414732144324734,-0.386384218345228,
-0.358442715127014,-0.3439725980329,-0.337412355992177,-0.308476667534375,
-0.301340440406708,-0.27349898470449,-0.24503506229541,-0.23372044216372,
-0.228077783746287,-0.199098898462337,-0.169542621789931,-0.139741118996361,
-0.123046348337536,-0.118258352302259,-0.114005782325404,-0.0834569890725602,
-0.0528735983342899,-0.0229279578859285,-0.00618295372576183,0.),
 .UNSPECIFIED.);
#1874=B_SPLINE_CURVE_WITH_KNOTS('',3,(#18995,#18996,#18997,#18998,#18999,
#19000,#19001,#19002,#19003,#19004,#19005,#19006,#19007,#19008,#19009,#19010,
#19011,#19012,#19013,#19014,#19015,#19016,#19017,#19018,#19019,#19020,#19021,
#19022,#19023,#19024,#19025,#19026,#19027,#19028,#19029,#19030,#19031,#19032,
#19033,#19034,#19035,#19036,#19037,#19038,#19039,#19040,#19041,#19042,#19043,
#19044,#19045,#19046,#19047,#19048,#19049,#19050,#19051,#19052,#19053,#19054,
#19055,#19056,#19057,#19058,#19059,#19060,#19061,#19062,#19063,#19064,#19065,
#19066,#19067,#19068,#19069,#19070,#19071,#19072,#19073,#19074,#19075,#19076,
#19077,#19078,#19079,#19080,#19081,#19082,#19083,#19084,#19085),
 .UNSPECIFIED.,.F.,.F.,(4,3,3,3,3,3,3,3,3,3,3,3,3,3,3,3,3,3,3,3,3,3,3,3,
3,3,3,3,3,3,4),(-0.566847306048112,-0.536668339194763,-0.506060306609139,
-0.497462971008878,-0.49048674636921,-0.460335880394182,-0.43688464809434,
-0.424130415052306,-0.418922833332638,-0.389496695041096,-0.360304026779685,
-0.332014506642465,-0.317192385480711,-0.312071032018094,-0.307326760176989,
-0.279357483073735,-0.27272602199545,-0.244230762652898,-0.214337412438226,
-0.205052717620921,-0.200811046971631,-0.172975225592022,-0.145198191377983,
-0.117889578720224,-0.103788876497136,-0.0993777838422393,-0.0726516837817966,
-0.0463548526568899,-0.0208998570126172,-0.00508396093552129,0.),
 .UNSPECIFIED.);
#1875=B_SPLINE_CURVE_WITH_KNOTS('',3,(#19087,#19088,#19089,#19090,#19091,
#19092,#19093,#19094,#19095,#19096,#19097),.UNSPECIFIED.,.F.,.F.,(4,1,1,
1,1,1,1,1,4),(15.7079632679489,15.852790517907,16.8512409318069,17.8496913457067,
18.8481417596065,19.8465921735064,20.8450425874062,21.843493001306,21.9911485751285),
 .UNSPECIFIED.);
#1876=B_SPLINE_CURVE_WITH_KNOTS('',3,(#19098,#19099,#19100,#19101,#19102,
#19103,#19104,#19105,#19106,#19107),.UNSPECIFIED.,.F.,.F.,(4,1,1,1,1,1,
1,4),(15.7079632679489,16.3953009547714,17.3937513686712,18.3922017825711,
19.3906521964709,20.3891026103707,21.3875530242705,21.9911485751285),
 .UNSPECIFIED.);
#1877=B_SPLINE_CURVE_WITH_KNOTS('',3,(#19556,#19557,#19558,#19559,#19560,
#19561,#19562,#19563,#19564,#19565,#19566,#19567,#19568,#19569,#19570,#19571,
#19572,#19573,#19574,#19575,#19576,#19577,#19578,#19579,#19580,#19581,#19582,
#19583,#19584,#19585,#19586,#19587,#19588,#19589,#19590,#19591,#19592,#19593,
#19594,#19595,#19596,#19597,#19598,#19599,#19600,#19601,#19602,#19603,#19604,
#19605,#19606,#19607,#19608,#19609,#19610,#19611,#19612,#19613,#19614,#19615,
#19616,#19617,#19618,#19619,#19620,#19621,#19622,#19623,#19624,#19625,#19626,
#19627,#19628,#19629,#19630,#19631,#19632,#19633,#19634,#19635,#19636,#19637,
#19638,#19639,#19640,#19641,#19642,#19643,#19644,#19645,#19646,#19647,#19648,
#19649,#19650,#19651,#19652),.UNSPECIFIED.,.F.,.F.,(4,3,3,3,3,3,3,3,3,3,
3,3,3,3,3,3,3,3,3,3,3,3,3,3,3,3,3,3,3,3,3,3,4),(0.,0.0253580839119621,0.0513883193661946,
0.0783500921775368,0.0901458677824991,0.0965510091518119,0.102699386274646,
0.130000465662217,0.157754532601719,0.185086524915523,0.19580591419694,
0.202109170553707,0.206420354259938,0.235022725853245,0.263529291896674,
0.267082501856933,0.294995261838824,0.306190778774865,0.311403784621555,
0.315731371826393,0.34382680331232,0.372961873868641,0.402415777646638,
0.414015416572459,0.420600208736835,0.426867850729504,0.456919286765161,
0.482861628469424,0.4929715795806,0.498519461182564,0.52960405738239,0.560688653582215,
0.566847306048152),.UNSPECIFIED.);
#1878=B_SPLINE_CURVE_WITH_KNOTS('',3,(#19653,#19654,#19655,#19656,#19657,
#19658,#19659,#19660,#19661,#19662,#19663,#19664,#19665,#19666,#19667,#19668,
#19669,#19670,#19671,#19672,#19673,#19674,#19675,#19676,#19677),
 .UNSPECIFIED.,.F.,.F.,(4,3,3,3,3,3,3,3,4),(-10.1321597128207,-9.98450413899828,
-8.98605372509846,-7.98760331119863,-6.9891528972988,-5.99070248339897,
-4.99225206949914,-3.99380165559931,-3.84897440564112),.UNSPECIFIED.);
#1879=B_SPLINE_CURVE_WITH_KNOTS('',3,(#20126,#20127,#20128,#20129,#20130,
#20131,#20132,#20133,#20134,#20135,#20136,#20137,#20138,#20139,#20140,#20141,
#20142,#20143,#20144,#20145,#20146,#20147),.UNSPECIFIED.,.F.,.F.,(4,3,3,
3,3,3,3,4),(7.59274844815663,7.98760331119864,8.98605372509847,9.9845041389983,
10.9829545528981,11.981404966798,12.9798553806978,13.8759337553362),
 .UNSPECIFIED.);
#1880=B_SPLINE_CURVE_WITH_KNOTS('',3,(#20148,#20149,#20150,#20151,#20152,
#20153,#20154,#20155,#20156,#20157,#20158,#20159,#20160,#20161,#20162,#20163,
#20164,#20165,#20166,#20167,#20168,#20169,#20170,#20171,#20172,#20173,#20174,
#20175,#20176,#20177,#20178,#20179,#20180,#20181,#20182,#20183,#20184,#20185,
#20186,#20187,#20188,#20189,#20190,#20191,#20192,#20193,#20194,#20195,#20196,
#20197,#20198,#20199,#20200,#20201,#20202,#20203,#20204,#20205,#20206,#20207,
#20208,#20209,#20210,#20211,#20212,#20213,#20214,#20215,#20216,#20217,#20218,
#20219,#20220,#20221,#20222,#20223,#20224,#20225,#20226,#20227,#20228,#20229,
#20230,#20231,#20232,#20233,#20234,#20235,#20236,#20237,#20238,#20239,#20240,
#20241),.UNSPECIFIED.,.F.,.F.,(4,3,3,3,3,3,3,3,3,3,3,3,3,3,3,3,3,3,3,3,
3,3,3,3,3,3,3,3,3,3,3,4),(0.,0.0297196497427133,0.0601024430505851,0.0895487561977697,
0.115314280201556,0.120671642680355,0.150435039105398,0.180035087607033,
0.20894455276229,0.221427550198096,0.230458612607052,0.234712819529639,
0.263250576278388,0.29115534663912,0.295672948228062,0.324625402415715,
0.334643829709069,0.339479004907797,0.343237704952895,0.371327052004073,
0.39947506248303,0.427228171302932,0.438025445099752,0.443793866239726,
0.448942908589349,0.476234910387191,0.498212935884146,0.507328822354416,
0.512108230143122,0.538127621259066,0.564147012375009,0.569248610399316),
 .UNSPECIFIED.);
#1881=B_SPLINE_CURVE_WITH_KNOTS('',3,(#20244,#20245,#20246,#20247,#20248,
#20249,#20250,#20251,#20252,#20253,#20254,#20255,#20256,#20257,#20258,#20259,
#20260,#20261,#20262,#20263,#20264,#20265,#20266,#20267,#20268,#20269,#20270,
#20271,#20272,#20273,#20274,#20275,#20276,#20277,#20278,#20279,#20280,#20281,
#20282,#20283,#20284,#20285,#20286,#20287,#20288,#20289,#20290,#20291,#20292,
#20293,#20294,#20295,#20296,#20297,#20298,#20299,#20300,#20301,#20302,#20303,
#20304,#20305,#20306,#20307,#20308,#20309,#20310,#20311,#20312,#20313,#20314,
#20315,#20316,#20317,#20318,#20319,#20320,#20321,#20322,#20323,#20324,#20325,
#20326,#20327,#20328,#20329,#20330,#20331,#20332,#20333,#20334),
 .UNSPECIFIED.,.F.,.F.,(4,3,3,3,3,3,3,3,3,3,3,3,3,3,3,3,3,3,3,3,3,3,3,3,
3,3,3,3,3,3,4),(-0.569248610399413,-0.543579424468409,-0.517280855913903,
-0.510431086725354,-0.504800591166774,-0.477739784666227,-0.455689866633776,
-0.448372084280305,-0.442463244683274,-0.414732125182678,-0.386384203988663,
-0.35844270327742,-0.343972580219404,-0.337412363788297,-0.308476675504046,
-0.301340440406619,-0.273498989180173,-0.245035069567214,-0.233720439206241,
-0.228077783767322,-0.199098902098819,-0.169542627253541,-0.139741124735967,
-0.123046353359691,-0.118258375487455,-0.114005833967889,-0.0834570417697634,
-0.0528736506474507,-0.0229280100403523,-0.00618295372576221,0.),
 .UNSPECIFIED.);
#1882=B_SPLINE_CURVE_WITH_KNOTS('',3,(#20335,#20336,#20337,#20338,#20339,
#20340,#20341,#20342,#20343,#20344,#20345,#20346,#20347,#20348,#20349,#20350,
#20351,#20352,#20353,#20354,#20355,#20356,#20357,#20358,#20359,#20360,#20361,
#20362,#20363,#20364,#20365,#20366,#20367,#20368,#20369,#20370,#20371,#20372,
#20373,#20374,#20375,#20376,#20377,#20378,#20379,#20380,#20381,#20382,#20383,
#20384,#20385,#20386,#20387,#20388,#20389,#20390,#20391,#20392,#20393,#20394,
#20395,#20396,#20397,#20398,#20399,#20400,#20401,#20402,#20403,#20404,#20405,
#20406,#20407,#20408,#20409,#20410,#20411,#20412,#20413,#20414,#20415,#20416,
#20417,#20418,#20419,#20420,#20421,#20422,#20423,#20424,#20425),
 .UNSPECIFIED.,.F.,.F.,(4,3,3,3,3,3,3,3,3,3,3,3,3,3,3,3,3,3,3,3,3,3,3,3,
3,3,3,3,3,3,4),(-0.566847306047958,-0.536668334620797,-0.506060300747489,
-0.49746296362483,-0.490486745065209,-0.460335879165694,-0.436884647019413,
-0.424130412363237,-0.418922832603944,-0.389496694866531,-0.360304026648761,
-0.332014507914833,-0.317192386434988,-0.312071036440509,-0.307326760696969,
-0.279357485335346,-0.272726021995452,-0.244230762694646,-0.214337412474756,
-0.205052718047108,-0.200811047279563,-0.172975225547944,-0.145198191396071,
-0.117889580168519,-0.103788877764395,-0.0993777847284473,-0.0726516854150365,
-0.046354856269949,-0.0208998643347332,-0.00508396093552485,0.),
 .UNSPECIFIED.);
#1883=B_SPLINE_CURVE_WITH_KNOTS('',3,(#20427,#20428,#20429,#20430,#20431,
#20432,#20433,#20434,#20435,#20436,#20437),.UNSPECIFIED.,.F.,.F.,(4,1,1,
1,1,1,1,1,4),(15.7079632679489,15.852790517907,16.8512409318069,17.8496913457067,
18.8481417596065,19.8465921735064,20.8450425874062,21.843493001306,21.9911485751285),
 .UNSPECIFIED.);
#1884=B_SPLINE_CURVE_WITH_KNOTS('',3,(#20438,#20439,#20440,#20441,#20442,
#20443,#20444,#20445,#20446,#20447),.UNSPECIFIED.,.F.,.F.,(4,1,1,1,1,1,
1,4),(15.7079632679489,16.3953009547714,17.3937513686712,18.3922017825711,
19.3906521964709,20.3891026103707,21.3875530242706,21.9911485751285),
 .UNSPECIFIED.);
#1885=B_SPLINE_CURVE_WITH_KNOTS('',3,(#20896,#20897,#20898,#20899,#20900,
#20901,#20902,#20903,#20904,#20905,#20906,#20907,#20908,#20909,#20910,#20911,
#20912,#20913,#20914,#20915,#20916,#20917,#20918,#20919,#20920,#20921,#20922,
#20923,#20924,#20925,#20926,#20927,#20928,#20929,#20930,#20931,#20932,#20933,
#20934,#20935,#20936,#20937,#20938,#20939,#20940,#20941,#20942,#20943,#20944,
#20945,#20946,#20947,#20948,#20949,#20950,#20951,#20952,#20953,#20954,#20955,
#20956,#20957,#20958,#20959,#20960,#20961,#20962,#20963,#20964,#20965,#20966,
#20967,#20968,#20969,#20970,#20971,#20972,#20973,#20974,#20975,#20976,#20977,
#20978,#20979,#20980,#20981,#20982,#20983,#20984,#20985,#20986,#20987,#20988,
#20989,#20990,#20991,#20992),.UNSPECIFIED.,.F.,.F.,(4,3,3,3,3,3,3,3,3,3,
3,3,3,3,3,3,3,3,3,3,3,3,3,3,3,3,3,3,3,3,3,3,4),(0.,0.0253580911802079,0.0513883332338855,
0.0783501043117711,0.0901458791583461,0.0965510147472824,0.102699384553703,
0.130000469046477,0.157754538584699,0.185086529402767,0.195805915508858,
0.202109172202035,0.206420354971663,0.23502272795396,0.263529291975222,
0.26708250185697,0.294995258577133,0.306190773496798,0.311403762156505,
0.315731366767556,0.343826793446803,0.372961861754818,0.402415764957967,
0.414015391046657,0.420600034660242,0.426867839516936,0.456919274359249,
0.482861619164976,0.492971552248951,0.498519433722844,0.5296040436525,0.560688653582156,
0.566847306048094),.UNSPECIFIED.);
#1886=B_SPLINE_CURVE_WITH_KNOTS('',3,(#20993,#20994,#20995,#20996,#20997,
#20998,#20999,#21000,#21001,#21002,#21003,#21004,#21005,#21006,#21007,#21008,
#21009,#21010,#21011,#21012,#21013,#21014,#21015,#21016,#21017),
 .UNSPECIFIED.,.F.,.F.,(4,3,3,3,3,3,3,3,4),(-10.1321597128207,-9.98450413899829,
-8.98605372509846,-7.98760331119863,-6.9891528972988,-5.99070248339897,
-4.99225206949914,-3.99380165559931,-3.84897440564113),.UNSPECIFIED.);
#1887=B_SPLINE_CURVE_WITH_KNOTS('',3,(#21466,#21467,#21468,#21469,#21470,
#21471,#21472,#21473,#21474,#21475,#21476,#21477,#21478,#21479,#21480,#21481,
#21482,#21483,#21484,#21485,#21486,#21487),.UNSPECIFIED.,.F.,.F.,(4,3,3,
3,3,3,3,4),(7.59274844815663,7.98760331119864,8.98605372509847,9.9845041389983,
10.9829545528981,11.981404966798,12.9798553806978,13.8759337553362),
 .UNSPECIFIED.);
#1888=B_SPLINE_CURVE_WITH_KNOTS('',3,(#21488,#21489,#21490,#21491,#21492,
#21493,#21494,#21495,#21496,#21497,#21498,#21499,#21500,#21501,#21502,#21503,
#21504,#21505,#21506,#21507,#21508,#21509,#21510,#21511,#21512,#21513,#21514,
#21515,#21516,#21517,#21518,#21519,#21520,#21521,#21522,#21523,#21524,#21525,
#21526,#21527,#21528,#21529,#21530,#21531,#21532,#21533,#21534,#21535,#21536,
#21537,#21538,#21539,#21540,#21541,#21542,#21543,#21544,#21545,#21546,#21547,
#21548,#21549,#21550,#21551,#21552,#21553,#21554,#21555,#21556,#21557,#21558,
#21559,#21560,#21561,#21562,#21563,#21564,#21565,#21566,#21567,#21568,#21569,
#21570,#21571,#21572,#21573,#21574,#21575,#21576,#21577,#21578,#21579,#21580,
#21581),.UNSPECIFIED.,.F.,.F.,(4,3,3,3,3,3,3,3,3,3,3,3,3,3,3,3,3,3,3,3,
3,3,3,3,3,3,3,3,3,3,3,4),(0.,0.0297196561791004,0.0601024527423554,0.0895487646780782,
0.115314287621836,0.120671644407955,0.15043504100573,0.180035087872894,
0.208944552961705,0.221427549682809,0.230458608873444,0.234712814484028,
0.263250569423067,0.29115533835926,0.295672948228138,0.324625402802554,
0.334643828946165,0.339479002351001,0.343237702251031,0.371327049518733,
0.399475060202899,0.427228167985078,0.438025437450442,0.443793859675948,
0.448942909106405,0.476234910274104,0.498212935799389,0.507328821201627,
0.5121082275177,0.538127619946472,0.564147012375243,0.569248610399555),
 .UNSPECIFIED.);
#1889=B_SPLINE_CURVE_WITH_KNOTS('',3,(#21751,#21752,#21753,#21754,#21755,
#21756,#21757,#21758,#21759,#21760,#21761,#21762,#21763,#21764,#21765,#21766,
#21767,#21768,#21769),.UNSPECIFIED.,.F.,.F.,(4,3,3,3,3,3,4),(95.5576018628658,
95.7627393059135,96.7602678403501,97.7577963747867,98.7553249092233,99.7528534436599,
100.750381978096),.UNSPECIFIED.);
#1890=B_SPLINE_CURVE_WITH_KNOTS('',3,(#21773,#21774,#21775,#21776),
 .UNSPECIFIED.,.F.,.F.,(4,4),(-98.735769112822,-98.0941628713861),
 .UNSPECIFIED.);
#1891=B_SPLINE_CURVE_WITH_KNOTS('',3,(#21780,#21781,#21782,#21783,#21784,
#21785,#21786,#21787,#21788,#21789,#21790,#21791,#21792,#21793,#21794,#21795,
#21796,#21797,#21798,#21799,#21800,#21801),.UNSPECIFIED.,.F.,.F.,(4,3,3,
3,3,3,3,4),(-98.0941628713861,-97.7577963747867,-96.7602678403501,-95.7627393059135,
-94.7652107714769,-93.7676822370403,-92.7701537026037,-91.8109775642065),
 .UNSPECIFIED.);
#1892=B_SPLINE_CURVE_WITH_KNOTS('',3,(#21806,#21807,#21808,#21809,#21810,
#21811,#21812,#21813,#21814,#21815,#21816,#21817,#21818,#21819,#21820,#21821,
#21822,#21823,#21824,#21825,#21826,#21827),.UNSPECIFIED.,.F.,.F.,(4,3,3,
3,3,3,3,4),(89.2744165556862,89.7775680992939,90.7750966337305,91.7726251681671,
92.7701537026037,93.7676822370403,94.7652107714769,95.5576018628658),
 .UNSPECIFIED.);
#1893=B_SPLINE_CURVE_WITH_KNOTS('',3,(#21828,#21829,#21830,#21831,#21832,
#21833,#21834,#21835,#21836,#21837,#21838,#21839,#21840,#21841,#21842,#21843,
#21844,#21845,#21846,#21847,#21848,#21849,#21850,#21851,#21852),
 .UNSPECIFIED.,.F.,.F.,(4,3,3,3,3,3,3,3,4),(-91.8109775642065,-91.7726251681671,
-90.7750966337305,-89.7775680992939,-88.7800395648573,-87.7825110304207,
-86.7849824959841,-85.7874539615475,-85.527792257027),.UNSPECIFIED.);
#1894=B_SPLINE_CURVE_WITH_KNOTS('',3,(#21857,#21858,#21859,#21860,#21861,
#21862,#21863,#21864,#21865,#21866,#21867,#21868,#21869,#21870,#21871,#21872,
#21873,#21874,#21875,#21876,#21877,#21878),.UNSPECIFIED.,.F.,.F.,(4,3,3,
3,3,3,3,4),(82.9912312485066,83.7923968926743,84.7899254271109,85.7874539615475,
86.7849824959841,87.7825110304207,88.7800395648573,89.2744165556862),
 .UNSPECIFIED.);
#1895=B_SPLINE_CURVE_WITH_KNOTS('',3,(#21879,#21880,#21881,#21882,#21883,
#21884,#21885,#21886,#21887,#21888,#21889,#21890,#21891,#21892,#21893,#21894,
#21895,#21896,#21897,#21898,#21899,#21900),.UNSPECIFIED.,.F.,.F.,(4,3,3,
3,3,3,3,4),(-85.527792257027,-84.7899254271109,-83.7923968926743,-82.7948683582377,
-81.7973398238011,-80.7998112893645,-79.8022827549279,-79.2446069498473),
 .UNSPECIFIED.);
#1896=B_SPLINE_CURVE_WITH_KNOTS('',3,(#21905,#21906,#21907,#21908,#21909,
#21910,#21911,#21912,#21913,#21914,#21915,#21916,#21917,#21918,#21919,#21920,
#21921,#21922,#21923,#21924,#21925,#21926,#21927,#21928,#21929),
 .UNSPECIFIED.,.F.,.F.,(4,3,3,3,3,3,3,3,4),(76.708045941327,76.8096971516181,
77.8072256860547,78.8047542204913,79.8022827549279,80.7998112893645,81.7973398238012,
82.7948683582377,82.9912312485066),.UNSPECIFIED.);
#1897=B_SPLINE_CURVE_WITH_KNOTS('',3,(#21930,#21931,#21932,#21933,#21934,
#21935,#21936,#21937,#21938,#21939,#21940,#21941,#21942,#21943,#21944,#21945,
#21946,#21947,#21948,#21949,#21950,#21951),.UNSPECIFIED.,.F.,.F.,(4,3,3,
3,3,3,3,4),(-79.2446069498473,-78.8047542204913,-77.8072256860547,-76.8096971516181,
-75.8121686171815,-74.8146400827449,-73.8171115483083,-72.9614216426677),
 .UNSPECIFIED.);
#1898=B_SPLINE_CURVE_WITH_KNOTS('',3,(#21956,#21957,#21958,#21959,#21960,
#21961,#21962,#21963,#21964,#21965,#21966,#21967,#21968,#21969,#21970,#21971,
#21972,#21973,#21974,#21975,#21976,#21977),.UNSPECIFIED.,.F.,.F.,(4,3,3,
3,3,3,3,4),(70.4248606341474,70.8245259449985,71.8220544794351,72.8195830138717,
73.8171115483083,74.8146400827449,75.8121686171815,76.708045941327),
 .UNSPECIFIED.);
#1899=B_SPLINE_CURVE_WITH_KNOTS('',3,(#21978,#21979,#21980,#21981,#21982,
#21983,#21984,#21985,#21986,#21987,#21988,#21989,#21990,#21991,#21992,#21993,
#21994,#21995,#21996,#21997,#21998,#21999,#22000,#22001,#22002),
 .UNSPECIFIED.,.F.,.F.,(4,3,3,3,3,3,3,3,4),(-72.9614216426677,-72.8195830138717,
-71.8220544794351,-70.8245259449985,-69.8269974105619,-68.8294688761253,
-67.8319403416887,-66.8344118072521,-66.6782363354882),.UNSPECIFIED.);
#1900=B_SPLINE_CURVE_WITH_KNOTS('',3,(#22007,#22008,#22009,#22010,#22011,
#22012,#22013,#22014,#22015,#22016,#22017,#22018,#22019,#22020,#22021,#22022,
#22023,#22024,#22025,#22026,#22027,#22028),.UNSPECIFIED.,.F.,.F.,(4,3,3,
3,3,3,3,4),(64.1416753269678,64.8393547383789,65.8368832728155,66.8344118072521,
67.8319403416887,68.8294688761253,69.8269974105619,70.4248606341474),
 .UNSPECIFIED.);
#1901=B_SPLINE_CURVE_WITH_KNOTS('',3,(#22029,#22030,#22031,#22032,#22033,
#22034,#22035,#22036,#22037,#22038,#22039,#22040,#22041,#22042,#22043,#22044,
#22045,#22046,#22047,#22048,#22049,#22050),.UNSPECIFIED.,.F.,.F.,(4,3,3,
3,3,3,3,4),(-66.6782363354882,-65.8368832728155,-64.8393547383789,-63.8418262039423,
-62.8442976695057,-61.8467691350691,-60.8492406006325,-60.3950510283086),
 .UNSPECIFIED.);
#1902=B_SPLINE_CURVE_WITH_KNOTS('',3,(#22055,#22056,#22057,#22058,#22059,
#22060,#22061,#22062,#22063,#22064,#22065,#22066,#22067,#22068,#22069,#22070,
#22071,#22072,#22073,#22074,#22075,#22076),.UNSPECIFIED.,.F.,.F.,(4,3,3,
3,3,3,3,4),(57.8584900197882,58.8541835317594,59.851712066196,60.8492406006326,
61.8467691350691,62.8442976695057,63.8418262039423,64.1416753269678),
 .UNSPECIFIED.);
#1903=B_SPLINE_CURVE_WITH_KNOTS('',3,(#22077,#22078,#22079,#22080,#22081,
#22082,#22083,#22084,#22085,#22086,#22087,#22088,#22089,#22090,#22091,#22092,
#22093,#22094,#22095,#22096,#22097,#22098),.UNSPECIFIED.,.F.,.F.,(4,3,3,
3,3,3,3,4),(-60.3950510283086,-59.851712066196,-58.8541835317593,-57.8566549973227,
-56.8591264628861,-55.8615979284495,-54.864069394013,-54.111865721129),
 .UNSPECIFIED.);
#1904=B_SPLINE_CURVE_WITH_KNOTS('',3,(#22103,#22104,#22105,#22106,#22107,
#22108,#22109,#22110,#22111,#22112,#22113,#22114,#22115,#22116,#22117,#22118,
#22119,#22120,#22121,#22122,#22123,#22124),.UNSPECIFIED.,.F.,.F.,(4,3,3,
3,3,3,3,4),(51.5753047126086,51.8714837907032,52.8690123251397,53.8665408595764,
54.864069394013,55.8615979284496,56.8591264628862,57.8584900197882),
 .UNSPECIFIED.);
#1905=B_SPLINE_CURVE_WITH_KNOTS('',3,(#22125,#22126,#22127,#22128,#22129,
#22130,#22131,#22132,#22133,#22134,#22135,#22136,#22137,#22138,#22139,#22140,
#22141,#22142,#22143,#22144,#22145,#22146,#22147,#22148,#22149),
 .UNSPECIFIED.,.F.,.F.,(4,3,3,3,3,3,3,3,4),(-54.111865721129,-53.8665408595764,
-52.8690123251397,-51.8714837907031,-50.8739552562666,-49.8764267218299,
-48.8788981873933,-47.8813696529567,-47.8286804139493),.UNSPECIFIED.);
#1906=B_SPLINE_CURVE_WITH_KNOTS('',3,(#22154,#22155,#22156,#22157,#22158,
#22159,#22160,#22161,#22162,#22163,#22164,#22165,#22166,#22167,#22168,#22169,
#22170,#22171,#22172,#22173,#22174,#22175),.UNSPECIFIED.,.F.,.F.,(4,3,3,
3,3,3,3,4),(45.292119405429,45.8863125840836,46.8838411185202,47.8813696529568,
48.8788981873934,49.87642672183,50.8739552562666,51.5753047126086),
 .UNSPECIFIED.);
#1907=B_SPLINE_CURVE_WITH_KNOTS('',3,(#22176,#22177,#22178,#22179,#22180,
#22181,#22182,#22183,#22184,#22185,#22186,#22187,#22188,#22189,#22190,#22191,
#22192,#22193,#22194,#22195,#22196,#22197),.UNSPECIFIED.,.F.,.F.,(4,3,3,
3,3,3,3,4),(-47.8286804139493,-46.8838411185201,-45.8863125840835,-44.888784049647,
-43.8912555152104,-42.8937269807738,-41.8961984463372,-41.5454951067698),
 .UNSPECIFIED.);
#1908=B_SPLINE_CURVE_WITH_KNOTS('',3,(#22202,#22203,#22204,#22205,#22206,
#22207,#22208,#22209,#22210,#22211,#22212,#22213,#22214,#22215,#22216,#22217,
#22218,#22219,#22220,#22221,#22222,#22223),.UNSPECIFIED.,.F.,.F.,(4,3,3,
3,3,3,3,4),(39.0089340982494,39.901141377464,40.8986699119006,41.8961984463372,
42.8937269807738,43.8912555152104,44.888784049647,45.292119405429),
 .UNSPECIFIED.);
#1909=B_SPLINE_CURVE_WITH_KNOTS('',3,(#22224,#22225,#22226,#22227,#22228,
#22229,#22230,#22231,#22232,#22233,#22234,#22235,#22236,#22237,#22238,#22239,
#22240,#22241,#22242,#22243,#22244,#22245),.UNSPECIFIED.,.F.,.F.,(4,3,3,
3,3,3,3,4),(-41.5454951067698,-40.8986699119006,-39.901141377464,-38.9036128430274,
-37.9060843085908,-36.9085557741542,-35.9110272397176,-35.2623097995902),
 .UNSPECIFIED.);
#1910=B_SPLINE_CURVE_WITH_KNOTS('',3,(#22250,#22251,#22252,#22253,#22254,
#22255,#22256,#22257,#22258,#22259,#22260,#22261,#22262,#22263,#22264,#22265,
#22266,#22267,#22268,#22269,#22270,#22271,#22272,#22273,#22274),
 .UNSPECIFIED.,.F.,.F.,(4,3,3,3,3,3,3,3,4),(32.7257487910698,32.9184416364078,
33.9159701708444,34.913498705281,35.9110272397176,36.9085557741542,37.9060843085908,
38.9036128430274,39.0089340982494),.UNSPECIFIED.);
#1911=B_SPLINE_CURVE_WITH_KNOTS('',3,(#22275,#22276,#22277,#22278,#22279,
#22280,#22281,#22282,#22283,#22284,#22285,#22286,#22287,#22288,#22289,#22290,
#22291,#22292,#22293,#22294,#22295,#22296),.UNSPECIFIED.,.F.,.F.,(4,3,3,
3,3,3,3,4),(-35.2623097995902,-34.913498705281,-33.9159701708444,-32.9184416364078,
-31.9209131019712,-30.9233845675346,-29.925856033098,-28.9791244924106),
 .UNSPECIFIED.);
#1912=B_SPLINE_CURVE_WITH_KNOTS('',3,(#22301,#22302,#22303,#22304,#22305,
#22306,#22307,#22308,#22309,#22310,#22311,#22312,#22313,#22314,#22315,#22316,
#22317,#22318,#22319,#22320,#22321,#22322),.UNSPECIFIED.,.F.,.F.,(4,3,3,
3,3,3,3,4),(26.4425634838902,26.9332704297882,27.9307989642248,28.9283274986614,
29.925856033098,30.9233845675346,31.9209131019712,32.7257487910698),
 .UNSPECIFIED.);
#1913=B_SPLINE_CURVE_WITH_KNOTS('',3,(#22323,#22324,#22325,#22326,#22327,
#22328,#22329,#22330,#22331,#22332,#22333,#22334,#22335,#22336,#22337,#22338,
#22339,#22340,#22341,#22342,#22343,#22344,#22345,#22346,#22347),
 .UNSPECIFIED.,.F.,.F.,(4,3,3,3,3,3,3,3,4),(-28.9791244924106,-28.9283274986614,
-27.9307989642248,-26.9332704297882,-25.9357418953516,-24.938213360915,
-23.9406848264784,-22.9431562920418,-22.695939185231),.UNSPECIFIED.);
#1914=B_SPLINE_CURVE_WITH_KNOTS('',3,(#22352,#22353,#22354,#22355,#22356,
#22357,#22358,#22359,#22360,#22361,#22362,#22363,#22364,#22365,#22366,#22367,
#22368,#22369,#22370,#22371,#22372,#22373),.UNSPECIFIED.,.F.,.F.,(4,3,3,
3,3,3,3,4),(20.1593781767107,20.9480992231686,21.9456277576052,22.9431562920418,
23.9406848264784,24.938213360915,25.9357418953516,26.4425634838902),
 .UNSPECIFIED.);
#1915=B_SPLINE_CURVE_WITH_KNOTS('',3,(#22374,#22375,#22376,#22377,#22378,
#22379,#22380,#22381,#22382,#22383,#22384,#22385,#22386,#22387,#22388,#22389,
#22390,#22391,#22392,#22393,#22394,#22395),.UNSPECIFIED.,.F.,.F.,(4,3,3,
3,3,3,3,4),(-22.695939185231,-21.9456277576052,-20.9480992231686,-19.950570688732,
-18.9530421542954,-17.9555136198588,-16.9579850854222,-16.4127538780514),
 .UNSPECIFIED.);
#1916=B_SPLINE_CURVE_WITH_KNOTS('',3,(#22400,#22401,#22402,#22403,#22404,
#22405,#22406,#22407,#22408,#22409,#22410,#22411,#22412,#22413,#22414,#22415,
#22416,#22417,#22418,#22419,#22420,#22421,#22422,#22423,#22424),
 .UNSPECIFIED.,.F.,.F.,(4,3,3,3,3,3,3,3,4),(13.8761928695311,13.9653994821124,
14.962928016549,15.9604565509856,16.9579850854222,17.9555136198588,18.9530421542954,
19.950570688732,20.1593781767107),.UNSPECIFIED.);
#1917=B_SPLINE_CURVE_WITH_KNOTS('',3,(#22425,#22426,#22427,#22428,#22429,
#22430,#22431,#22432,#22433,#22434,#22435,#22436,#22437,#22438,#22439,#22440,
#22441,#22442,#22443,#22444,#22445,#22446),.UNSPECIFIED.,.F.,.F.,(4,3,3,
3,3,3,3,4),(-16.4127538780514,-15.9604565509856,-14.962928016549,-13.9653994821124,
-12.9678709476758,-11.9703424132392,-10.9728138788026,-10.1295685708718),
 .UNSPECIFIED.);
#1918=B_SPLINE_CURVE_WITH_KNOTS('',3,(#22452,#22453,#22454,#22455,#22456,
#22457,#22458,#22459,#22460,#22461,#22462,#22463,#22464),.UNSPECIFIED.,
 .F.,.F.,(4,3,3,3,4),(-3.84638326369226,-2.9925856033098,-1.9950570688732,
-0.997528534436599,0.),.UNSPECIFIED.);
#1919=B_SPLINE_CURVE_WITH_KNOTS('',3,(#22467,#22468,#22469,#22470,#22471,
#22472,#22473,#22474,#22475,#22476,#22477,#22478,#22479,#22480,#22481,#22482,
#22483,#22484,#22485),.UNSPECIFIED.,.F.,.F.,(4,3,3,3,3,3,4),(2.01461286527445,
2.9925856033098,3.9901141377464,4.987642672183,5.9851712066196,6.9826997410562,
7.59300756235149),.UNSPECIFIED.);
#1920=B_SPLINE_CURVE_WITH_KNOTS('',3,(#22491,#22492,#22493,#22494,#22495,
#22496),.UNSPECIFIED.,.F.,.F.,(4,1,1,4),(109.955742875643,110.61690491348,
111.614433447917,112.611961982353),.UNSPECIFIED.);
#1921=B_SPLINE_CURVE_WITH_KNOTS('',3,(#22499,#22500,#22501,#22502,#22503,
#22504,#22505),.UNSPECIFIED.,.F.,.F.,(4,1,1,1,4),(109.955742875643,110.16088031869,
111.158408853127,112.155937387564,113.133910125599),.UNSPECIFIED.);
#1922=B_SPLINE_CURVE_WITH_KNOTS('',3,(#22510,#22511,#22512,#22513,#22514,
#22515,#22516,#22517,#22518,#22519),.UNSPECIFIED.,.F.,.F.,(4,1,1,1,1,1,
1,4),(103.672557568463,104.63173370686,105.629262241297,106.626790775734,
107.62431931017,108.621847844607,109.619376379043,109.955742875643),
 .UNSPECIFIED.);
#1923=B_SPLINE_CURVE_WITH_KNOTS('',3,(#22520,#22521,#22522,#22523,#22524,
#22525,#22526,#22527,#22528,#22529),.UNSPECIFIED.,.F.,.F.,(4,1,1,1,1,1,
1,4),(103.672557568463,104.175709112071,105.173237646507,106.170766180944,
107.168294715381,108.165823249817,109.163351784254,109.955742875643),
 .UNSPECIFIED.);
#1924=B_SPLINE_CURVE_WITH_KNOTS('',3,(#22534,#22535,#22536,#22537,#22538,
#22539,#22540,#22541,#22542,#22543,#22544),.UNSPECIFIED.,.F.,.F.,(4,1,1,
1,1,1,1,1,4),(97.3893722612836,97.6490339658042,98.6465625002407,99.6440910346773,
100.641619569114,101.639148103551,102.636676637987,103.634205172424,103.672557568463),
 .UNSPECIFIED.);
#1925=B_SPLINE_CURVE_WITH_KNOTS('',3,(#22545,#22546,#22547,#22548,#22549,
#22550,#22551,#22552,#22553,#22554),.UNSPECIFIED.,.F.,.F.,(4,1,1,1,1,1,
1,4),(97.3893722612836,98.1905379054512,99.1880664398878,100.185594974324,
101.183123508761,102.180652043198,103.178180577634,103.672557568463),
 .UNSPECIFIED.);
#1926=B_SPLINE_CURVE_WITH_KNOTS('',3,(#22559,#22560,#22561,#22562,#22563,
#22564,#22565,#22566,#22567,#22568),.UNSPECIFIED.,.F.,.F.,(4,1,1,1,1,1,
1,4),(91.106186954104,91.6638627591846,92.6613912936212,93.6589198280577,
94.6564483624943,95.6539768969309,96.6515054313676,97.3893722612836),
 .UNSPECIFIED.);
#1927=B_SPLINE_CURVE_WITH_KNOTS('',3,(#22569,#22570,#22571,#22572,#22573,
#22574,#22575,#22576,#22577,#22578,#22579),.UNSPECIFIED.,.F.,.F.,(4,1,1,
1,1,1,1,1,4),(91.106186954104,91.207838164395,92.2053666988316,93.2028952332682,
94.2004237677048,95.1979523021414,96.195480836578,97.1930093710146,97.3893722612836),
 .UNSPECIFIED.);
#1928=B_SPLINE_CURVE_WITH_KNOTS('',3,(#22584,#22585,#22586,#22587,#22588,
#22589,#22590,#22591,#22592,#22593),.UNSPECIFIED.,.F.,.F.,(4,1,1,1,1,1,
1,4),(84.8230016469244,85.678691552565,86.6762200870016,87.6737486214382,
88.6712771558748,89.6688056903114,90.666334224748,91.106186954104),
 .UNSPECIFIED.);
#1929=B_SPLINE_CURVE_WITH_KNOTS('',3,(#22594,#22595,#22596,#22597,#22598,
#22599,#22600,#22601,#22602,#22603),.UNSPECIFIED.,.F.,.F.,(4,1,1,1,1,1,
1,4),(84.8230016469244,85.2226669577754,86.220195492212,87.2177240266486,
88.2152525610852,89.2127810955218,90.2103096299584,91.106186954104),
 .UNSPECIFIED.);
#1930=B_SPLINE_CURVE_WITH_KNOTS('',3,(#22608,#22609,#22610,#22611,#22612,
#22613,#22614,#22615,#22616,#22617,#22618),.UNSPECIFIED.,.F.,.F.,(4,1,1,
1,1,1,1,1,4),(78.5398163397448,78.6959918115088,79.6935203459454,80.691048880382,
81.6885774148186,82.6861059492552,83.6836344836918,84.6811630181284,84.8230016469244),
 .UNSPECIFIED.);
#1931=B_SPLINE_CURVE_WITH_KNOTS('',3,(#22619,#22620,#22621,#22622,#22623,
#22624,#22625,#22626,#22627,#22628),.UNSPECIFIED.,.F.,.F.,(4,1,1,1,1,1,
1,4),(78.5398163397448,79.2374957511558,80.2350242855924,81.232552820029,
82.2300813544657,83.2276098889023,84.2251384233388,84.8230016469244),
 .UNSPECIFIED.);
#1932=B_SPLINE_CURVE_WITH_KNOTS('',3,(#22633,#22634,#22635,#22636,#22637,
#22638,#22639,#22640,#22641,#22642),.UNSPECIFIED.,.F.,.F.,(4,1,1,1,1,1,
1,4),(72.2566310325652,72.7108206048892,73.7083491393258,74.7058776737624,
75.703406208199,76.7009347426356,77.6984632770722,78.5398163397448),
 .UNSPECIFIED.);
#1933=B_SPLINE_CURVE_WITH_KNOTS('',3,(#22643,#22644,#22645,#22646,#22647,
#22648,#22649,#22650,#22651,#22652),.UNSPECIFIED.,.F.,.F.,(4,1,1,1,1,1,
1,4),(72.2566310325652,73.2523245445363,74.2498530789728,75.2473816134095,
76.244910147846,77.2424386822827,78.2399672167193,78.5398163397448),
 .UNSPECIFIED.);
#1934=B_SPLINE_CURVE_WITH_KNOTS('',3,(#22657,#22658,#22659,#22660,#22661,
#22662,#22663,#22664,#22665,#22666),.UNSPECIFIED.,.F.,.F.,(4,1,1,1,1,1,
1,4),(65.9734457253856,66.7256493982696,67.7231779327062,68.7207064671428,
69.7182350015794,70.715763536016,71.7132920704526,72.2566310325652),
 .UNSPECIFIED.);
#1935=B_SPLINE_CURVE_WITH_KNOTS('',3,(#22667,#22668,#22669,#22670,#22671,
#22672,#22673,#22674,#22675,#22676,#22677),.UNSPECIFIED.,.F.,.F.,(4,1,1,
1,1,1,1,1,4),(65.9734457253856,66.2696248034801,67.2671533379167,68.2646818723533,
69.2622104067898,70.2597389412265,71.2572674756631,72.2547960100997,72.2566310325652),
 .UNSPECIFIED.);
#1936=B_SPLINE_CURVE_WITH_KNOTS('',3,(#22682,#22683,#22684,#22685,#22686,
#22687,#22688,#22689,#22690,#22691,#22692),.UNSPECIFIED.,.F.,.F.,(4,1,1,
1,1,1,1,1,4),(59.690260418206,59.7429496572134,60.74047819165,61.7380067260866,
62.7355352605232,63.7330637949598,64.7305923293964,65.728120863833,65.9734457253856),
 .UNSPECIFIED.);
#1937=B_SPLINE_CURVE_WITH_KNOTS('',3,(#22693,#22694,#22695,#22696,#22697,
#22698,#22699,#22700,#22701,#22702),.UNSPECIFIED.,.F.,.F.,(4,1,1,1,1,1,
1,4),(59.690260418206,60.2844535968605,61.2819821312971,62.2795106657337,
63.2770392001703,64.2745677346069,65.2720962690435,65.9734457253856),
 .UNSPECIFIED.);
#1938=B_SPLINE_CURVE_WITH_KNOTS('',3,(#22707,#22708,#22709,#22710,#22711,
#22712,#22713,#22714,#22715,#22716),.UNSPECIFIED.,.F.,.F.,(4,1,1,1,1,1,
1,4),(53.4070751110264,53.7577784505938,54.7553069850304,55.752835519467,
56.7503640539036,57.7478925883402,58.7454211227768,59.690260418206),
 .UNSPECIFIED.);
#1939=B_SPLINE_CURVE_WITH_KNOTS('',3,(#22717,#22718,#22719,#22720,#22721,
#22722,#22723,#22724,#22725,#22726),.UNSPECIFIED.,.F.,.F.,(4,1,1,1,1,1,
1,4),(53.4070751110264,54.2992823902409,55.2968109246775,56.2943394591141,
57.2918679935507,58.2893965279873,59.2869250624239,59.690260418206),
 .UNSPECIFIED.);
#1940=B_SPLINE_CURVE_WITH_KNOTS('',3,(#22731,#22732,#22733,#22734,#22735,
#22736,#22737,#22738,#22739,#22740),.UNSPECIFIED.,.F.,.F.,(4,1,1,1,1,1,
1,4),(47.1238898038468,47.7726072439742,48.7701357784108,49.7676643128474,
50.765192847284,51.7627213817206,52.7602499161572,53.4070751110264),
 .UNSPECIFIED.);
#1941=B_SPLINE_CURVE_WITH_KNOTS('',3,(#22741,#22742,#22743,#22744,#22745,
#22746,#22747,#22748,#22749,#22750,#22751),.UNSPECIFIED.,.F.,.F.,(4,1,1,
1,1,1,1,1,4),(47.1238898038468,47.3165826491847,48.3141111836213,49.3116397180579,
50.3091682524945,51.3066967869311,52.3042253213677,53.3017538558043,53.4070751110264),
 .UNSPECIFIED.);
#1942=B_SPLINE_CURVE_WITH_KNOTS('',3,(#22756,#22757,#22758,#22759,#22760,
#22761,#22762,#22763,#22764,#22765),.UNSPECIFIED.,.F.,.F.,(4,1,1,1,1,1,
1,4),(40.8407044966673,41.7874360373546,42.7849645717912,43.7824931062278,
44.7800216406644,45.777550175101,46.7750787095376,47.1238898038468),
 .UNSPECIFIED.);
#1943=B_SPLINE_CURVE_WITH_KNOTS('',3,(#22766,#22767,#22768,#22769,#22770,
#22771,#22772,#22773,#22774,#22775),.UNSPECIFIED.,.F.,.F.,(4,1,1,1,1,1,
1,4),(40.8407044966673,41.3314114425651,42.3289399770017,43.3264685114383,
44.3239970458749,45.3215255803115,46.3190541147481,47.1238898038468),
 .UNSPECIFIED.);
#1944=B_SPLINE_CURVE_WITH_KNOTS('',3,(#22780,#22781,#22782,#22783,#22784,
#22785,#22786,#22787,#22788,#22789,#22790),.UNSPECIFIED.,.F.,.F.,(4,1,1,
1,1,1,1,1,4),(34.5575191894876,34.8047362962984,35.802264830735,36.7997933651716,
37.7973218996082,38.7948504340448,39.7923789684814,40.789907502918,40.8407044966673),
 .UNSPECIFIED.);
#1945=B_SPLINE_CURVE_WITH_KNOTS('',3,(#22791,#22792,#22793,#22794,#22795,
#22796,#22797,#22798,#22799,#22800),.UNSPECIFIED.,.F.,.F.,(4,1,1,1,1,1,
1,4),(34.5575191894876,35.3462402359455,36.3437687703821,37.3412973048187,
38.3388258392553,39.3363543736919,40.3338829081285,40.8407044966673),
 .UNSPECIFIED.);
#1946=B_SPLINE_CURVE_WITH_KNOTS('',3,(#22805,#22806,#22807,#22808,#22809,
#22810,#22811,#22812,#22813,#22814),.UNSPECIFIED.,.F.,.F.,(4,1,1,1,1,1,
1,4),(28.2743338823081,28.8195650896788,29.8170936241154,30.814622158552,
31.8121506929886,32.8096792274252,33.8072077618618,34.5575191894876),
 .UNSPECIFIED.);
#1947=B_SPLINE_CURVE_WITH_KNOTS('',3,(#22815,#22816,#22817,#22818,#22819,
#22820,#22821,#22822,#22823,#22824,#22825),.UNSPECIFIED.,.F.,.F.,(4,1,1,
1,1,1,1,1,4),(28.2743338823081,28.3635404948893,29.3610690293259,30.3585975637625,
31.3561260981991,32.3536546326357,33.3511831670723,34.3487117015089,34.5575191894876),
 .UNSPECIFIED.);
#1948=B_SPLINE_CURVE_WITH_KNOTS('',3,(#22830,#22831,#22832,#22833,#22834,
#22835,#22836,#22837,#22838,#22839),.UNSPECIFIED.,.F.,.F.,(4,1,1,1,1,1,
1,4),(21.9911485751284,22.8343938830592,23.8319224174958,24.8294509519324,
25.826979486369,26.8245080208056,27.8220365552422,28.2743338823081),
 .UNSPECIFIED.);
#1949=B_SPLINE_CURVE_WITH_KNOTS('',3,(#22840,#22841,#22842,#22843,#22844,
#22845,#22846,#22847,#22848,#22849),.UNSPECIFIED.,.F.,.F.,(4,1,1,1,1,1,
1,4),(21.9911485751284,22.3783692882697,23.3758978227063,24.3734263571429,
25.3709548915795,26.3684834260161,27.3660119604527,28.2743338823081),
 .UNSPECIFIED.);
#1950=B_SPLINE_CURVE_WITH_KNOTS('',3,(#22855,#22856,#22857,#22858,#22859),
 .UNSPECIFIED.,.F.,.F.,(4,1,4),(14.3981410127769,15.3956695472135,15.7079632679489),
 .UNSPECIFIED.);
#1951=B_SPLINE_CURVE_WITH_KNOTS('',3,(#22862,#22863,#22864,#22865,#22866),
 .UNSPECIFIED.,.F.,.F.,(4,1,4),(13.8761928695311,14.8541656075664,15.7079632679489),
 .UNSPECIFIED.);
#1952=B_SPLINE_CURVE_WITH_KNOTS('',3,(#22868,#22869,#22870,#22871,#22872,
#22873,#22874,#22875,#22876,#22877,#22878,#22879,#22880,#22881,#22882,#22883,
#22884,#22885,#22886,#22887,#22888,#22889,#22890,#22891,#22892,#22893,#22894,
#22895,#22896,#22897,#22898,#22899,#22900,#22901,#22902,#22903,#22904,#22905,
#22906,#22907,#22908,#22909,#22910,#22911,#22912,#22913,#22914,#22915,#22916,
#22917,#22918,#22919,#22920,#22921,#22922,#22923,#22924,#22925,#22926,#22927,
#22928,#22929,#22930,#22931,#22932,#22933,#22934,#22935,#22936,#22937,#22938,
#22939,#22940,#22941,#22942,#22943,#22944,#22945,#22946,#22947,#22948,#22949,
#22950,#22951,#22952,#22953,#22954,#22955),.UNSPECIFIED.,.F.,.F.,(4,3,3,
3,3,3,3,3,3,3,3,3,3,3,3,3,3,3,3,3,3,3,3,3,3,3,3,3,3,4),(-0.378621596831403,
-0.359793800533641,-0.347850189670991,-0.339636048942975,-0.335335774136304,
-0.31546051317345,-0.301132643095686,-0.297156907494375,-0.293211954051928,
-0.272807042011262,-0.252109806400788,-0.239291742938424,-0.228786234997388,
-0.224498858881779,-0.203194502850499,-0.200837552551333,-0.180352825937995,
-0.158313007596234,-0.154345292986098,-0.150812110310244,-0.129430920910395,
-0.107597661495996,-0.0856310553157248,-0.0802130557452004,-0.0759476002900926,
-0.0534004481199611,-0.0308282090279777,-0.00877005394723412,-0.00403427920391026,
0.),.UNSPECIFIED.);
#1953=B_SPLINE_CURVE_WITH_KNOTS('',3,(#22956,#22957,#22958,#22959,#22960,
#22961,#22962,#22963,#22964,#22965,#22966,#22967,#22968,#22969,#22970,#22971,
#22972,#22973,#22974,#22975,#22976,#22977,#22978,#22979,#22980,#22981,#22982,
#22983,#22984,#22985,#22986,#22987,#22988,#22989,#22990,#22991,#22992,#22993,
#22994,#22995,#22996,#22997,#22998,#22999,#23000,#23001,#23002,#23003,#23004,
#23005,#23006,#23007,#23008,#23009,#23010,#23011,#23012,#23013,#23014,#23015,
#23016,#23017,#23018,#23019,#23020,#23021,#23022,#23023,#23024,#23025,#23026,
#23027,#23028,#23029,#23030,#23031,#23032,#23033,#23034,#23035,#23036,#23037,
#23038,#23039,#23040),.UNSPECIFIED.,.F.,.F.,(4,3,3,3,3,3,3,3,3,3,3,3,3,
3,3,3,3,3,3,3,3,3,3,3,3,3,3,3,4),(-0.376940817211647,-0.354631959429703,
-0.332910822711019,-0.32806220569962,-0.305813663335352,-0.290194813628462,
-0.284256552410819,-0.278600734522432,-0.256917979000876,-0.235701442818543,
-0.214949892844509,-0.208195692337994,-0.204402258299287,-0.183827120255531,
-0.180862865680235,-0.159880225304417,-0.140305799915047,-0.136023059343962,
-0.132589312410188,-0.11212985906865,-0.0917656064462646,-0.0718387373507178,
-0.0676299187791264,-0.0636628529112296,-0.044105741114238,-0.024921443999485,
-0.00636112761058051,-0.00328482218945467,0.),.UNSPECIFIED.);
#1954=B_SPLINE_CURVE_WITH_KNOTS('',3,(#23042,#23043,#23044,#23045,#23046,
#23047,#23048,#23049,#23050,#23051,#23052),.UNSPECIFIED.,.F.,.F.,(4,1,1,
1,1,1,1,1,4),(15.7079632679489,15.851694142003,16.8492226764396,17.8467512108762,
18.8442797453128,19.8418082797494,20.839336814186,21.8368653486226,21.9911485751284),
 .UNSPECIFIED.);
#1955=B_SPLINE_CURVE_WITH_KNOTS('',3,(#23053,#23054,#23055,#23056,#23057,
#23058,#23059,#23060,#23061,#23062),.UNSPECIFIED.,.F.,.F.,(4,1,1,1,1,1,
1,4),(15.7079632679489,16.3931980816501,17.3907266160867,18.3882551505233,
19.3857836849599,20.3833122193965,21.3808407538331,21.9911485751284),
 .UNSPECIFIED.);
#1956=B_SPLINE_CURVE_WITH_KNOTS('',3,(#23479,#23480,#23481,#23482,#23483,
#23484,#23485,#23486,#23487,#23488,#23489,#23490,#23491,#23492,#23493,#23494,
#23495,#23496,#23497,#23498,#23499,#23500,#23501,#23502,#23503,#23504,#23505,
#23506,#23507,#23508,#23509,#23510,#23511,#23512,#23513,#23514,#23515,#23516,
#23517,#23518,#23519,#23520,#23521,#23522,#23523,#23524,#23525,#23526,#23527,
#23528,#23529,#23530,#23531,#23532,#23533,#23534,#23535,#23536,#23537,#23538,
#23539,#23540,#23541,#23542,#23543,#23544,#23545,#23546,#23547,#23548,#23549,
#23550,#23551,#23552,#23553,#23554,#23555,#23556,#23557,#23558,#23559,#23560),
 .UNSPECIFIED.,.F.,.F.,(4,3,3,3,3,3,3,3,3,3,3,3,3,3,3,3,3,3,3,3,3,3,3,3,
3,3,3,4),(0.,0.0186013309220082,0.0384258187432639,0.0557722455868627,0.064476526623233,
0.0684519336897636,0.0885088376090689,0.108919913995898,0.125989243869937,
0.133854361750648,0.137287827509053,0.158362305677327,0.177197233492054,
0.197723029954501,0.205648563033172,0.209124559961607,0.230127910462039,
0.251618950585589,0.268076130837863,0.278319720735245,0.284044100051126,
0.30631294997178,0.322965504893635,0.328171461506484,0.333183430590058,
0.355704845535606,0.372923169659198,0.376940817211655),.UNSPECIFIED.);
#1957=B_SPLINE_CURVE_WITH_KNOTS('',3,(#23561,#23562,#23563,#23564,#23565,
#23566,#23567,#23568,#23569,#23570,#23571,#23572,#23573,#23574,#23575,#23576,
#23577,#23578,#23579,#23580,#23581,#23582,#23583,#23584,#23585),
 .UNSPECIFIED.,.F.,.F.,(4,3,3,3,3,3,3,3,4),(-10.1295685708718,-9.97528534436599,
-8.97775680992939,-7.98022827549279,-6.98269974105619,-5.98517120661959,
-4.98764267218299,-3.9901141377464,-3.84638326369226),.UNSPECIFIED.);
#1958=B_SPLINE_CURVE_WITH_KNOTS('',3,(#24002,#24003,#24004,#24005,#24006,
#24007,#24008,#24009,#24010,#24011,#24012,#24013,#24014,#24015,#24016,#24017,
#24018,#24019,#24020,#24021,#24022,#24023),.UNSPECIFIED.,.F.,.F.,(4,3,3,
3,3,3,3,4),(7.59300756235149,7.98022827549279,8.97775680992939,9.97528534436599,
10.9728138788026,11.9703424132392,12.9678709476758,13.8761928695311),
 .UNSPECIFIED.);
#1959=B_SPLINE_CURVE_WITH_KNOTS('',3,(#24024,#24025,#24026,#24027,#24028,
#24029,#24030,#24031,#24032,#24033,#24034,#24035,#24036,#24037,#24038,#24039,
#24040,#24041,#24042,#24043,#24044,#24045,#24046,#24047,#24048,#24049,#24050,
#24051,#24052,#24053,#24054,#24055,#24056,#24057,#24058,#24059,#24060,#24061,
#24062,#24063,#24064,#24065,#24066,#24067,#24068,#24069,#24070,#24071,#24072,
#24073,#24074,#24075,#24076,#24077,#24078,#24079,#24080,#24081,#24082,#24083,
#24084,#24085,#24086,#24087,#24088,#24089,#24090,#24091,#24092,#24093,#24094,
#24095,#24096,#24097,#24098,#24099,#24100,#24101,#24102,#24103,#24104,#24105,
#24106,#24107,#24108),.UNSPECIFIED.,.F.,.F.,(4,3,3,3,3,3,3,3,3,3,3,3,3,
3,3,3,3,3,3,3,3,3,3,3,3,3,3,3,4),(0.,0.0219693271129621,0.0445470856655639,
0.0636231399133006,0.0720978574378349,0.0767563405636669,0.0810490577745036,
0.102995570811128,0.124770875307109,0.142867036392196,0.150422875677093,
0.153918682854505,0.157566935291381,0.178336708531301,0.197155519647457,
0.219426672701596,0.224327949631498,0.229401226278881,0.250066427413625,
0.27072708362855,0.285673099166475,0.296886737298637,0.300621606934625,
0.320392720001204,0.334297633865279,0.338764463536532,0.35778760385162,
0.375324744080566,0.378621596831418),.UNSPECIFIED.);
#1960=B_SPLINE_CURVE_WITH_KNOTS('',3,(#24328,#24329,#24330,#24331,#24332,
#24333,#24334,#24335,#24336,#24337),.UNSPECIFIED.,.F.,.F.,(4,3,3,4),(-4.09254174883832,
-3.98935377563313,-2.99201533172485,-2.06514013327812),.UNSPECIFIED.);
#1961=B_SPLINE_CURVE_WITH_KNOTS('',3,(#24340,#24341,#24342,#24343,#24344,
#24345,#24346),.UNSPECIFIED.,.F.,.F.,(4,3,4),(0.,0.998359650364244,1.11419103802955),
 .UNSPECIFIED.);
#1962=B_SPLINE_CURVE_WITH_KNOTS('',3,(#24351,#24352,#24353,#24354,#24355,
#24356,#24357,#24358,#24359,#24360,#24361,#24362,#24363,#24364,#24365,#24366,
#24367,#24368,#24369,#24370,#24371,#24372),.UNSPECIFIED.,.F.,.F.,(4,3,3,
3,3,3,3,4),(-10.3757270560179,-9.97338443908282,-8.97604599517454,-7.97870755126626,
-6.98136910735798,-5.98403066344969,-4.98669221954141,-4.09254174883832),
 .UNSPECIFIED.);
#1963=B_SPLINE_CURVE_WITH_KNOTS('',3,(#24373,#24374,#24375,#24376,#24377,
#24378,#24379,#24380,#24381,#24382,#24383,#24384,#24385,#24386,#24387,#24388,
#24389,#24390,#24391,#24392,#24393,#24394),.UNSPECIFIED.,.F.,.F.,(4,3,3,
3,3,3,3,4),(1.11419103802955,1.99671930072849,2.99507895109274,3.99343860145699,
4.99179825182123,5.99015790218548,6.98851755254973,7.39737634520914),
 .UNSPECIFIED.);
#1964=B_SPLINE_CURVE_WITH_KNOTS('',3,(#24399,#24400,#24401,#24402,#24403,
#24404,#24405,#24406,#24407,#24408,#24409,#24410,#24411,#24412,#24413,#24414,
#24415,#24416,#24417,#24418,#24419,#24420),.UNSPECIFIED.,.F.,.F.,(4,3,3,
3,3,3,3,4),(-16.6589123631975,-15.9574151025325,-14.9600766586242,-13.962738214716,
-12.9653997708077,-11.9680613268994,-10.9707228829911,-10.3757270560179),
 .UNSPECIFIED.);
#1965=B_SPLINE_CURVE_WITH_KNOTS('',3,(#24421,#24422,#24423,#24424,#24425,
#24426,#24427,#24428,#24429,#24430,#24431,#24432,#24433,#24434,#24435,#24436,
#24437,#24438,#24439,#24440,#24441,#24442),.UNSPECIFIED.,.F.,.F.,(4,3,3,
3,3,3,3,4),(7.39737634520914,7.98687720291397,8.98523685327822,9.98359650364247,
10.9819561540067,11.980315804371,12.9786754547352,13.6805616523887),
 .UNSPECIFIED.);
#1966=B_SPLINE_CURVE_WITH_KNOTS('',3,(#24447,#24448,#24449,#24450,#24451,
#24452,#24453,#24454,#24455,#24456,#24457,#24458,#24459,#24460,#24461,#24462,
#24463,#24464,#24465,#24466,#24467,#24468,#24469,#24470,#24471),
 .UNSPECIFIED.,.F.,.F.,(4,3,3,3,3,3,3,3,4),(-22.9420976703771,-22.9387842098905,
-21.9414457659822,-20.9441073220739,-19.9467688781656,-18.9494304342574,
-17.9520919903491,-16.9547535464408,-16.6589123631975),.UNSPECIFIED.);
#1967=B_SPLINE_CURVE_WITH_KNOTS('',3,(#24472,#24473,#24474,#24475,#24476,
#24477,#24478,#24479,#24480,#24481,#24482,#24483,#24484,#24485,#24486,#24487,
#24488,#24489,#24490,#24491,#24492,#24493),.UNSPECIFIED.,.F.,.F.,(4,3,3,
3,3,3,3,4),(13.6805616523887,13.9770351050995,14.9753947554637,15.973754405828,
16.9721140561922,17.9704737065565,18.9688333569207,19.9637469595683),
 .UNSPECIFIED.);
#1968=B_SPLINE_CURVE_WITH_KNOTS('',3,(#24498,#24499,#24500,#24501,#24502,
#24503,#24504,#24505,#24506,#24507,#24508,#24509,#24510,#24511,#24512,#24513,
#24514,#24515,#24516,#24517,#24518,#24519),.UNSPECIFIED.,.F.,.F.,(4,3,3,
3,3,3,3,4),(-29.2252829775567,-28.9228148733402,-27.9254764294319,-26.9281379855236,
-25.9307995416153,-24.9334610977071,-23.9361226537988,-22.9420976703771),
 .UNSPECIFIED.);
#1969=B_SPLINE_CURVE_WITH_KNOTS('',3,(#24520,#24521,#24522,#24523,#24524,
#24525,#24526,#24527,#24528,#24529,#24530,#24531,#24532,#24533,#24534,#24535,
#24536,#24537,#24538,#24539,#24540,#24541,#24542,#24543,#24544),
 .UNSPECIFIED.,.F.,.F.,(4,3,3,3,3,3,3,3,4),(19.9637469595683,19.967193007285,
20.9655526576492,21.9639123080134,22.9622719583777,23.9606316087419,24.9589912591062,
25.9573509094704,26.2469322667479),.UNSPECIFIED.);
#1970=B_SPLINE_CURVE_WITH_KNOTS('',3,(#24549,#24550,#24551,#24552,#24553,
#24554,#24555,#24556,#24557,#24558,#24559,#24560,#24561,#24562,#24563,#24564,
#24565,#24566,#24567,#24568,#24569,#24570),.UNSPECIFIED.,.F.,.F.,(4,3,3,
3,3,3,3,4),(-35.5084682847363,-34.9068455367899,-33.9095070928816,-32.9121686489733,
-31.914830205065,-30.9174917611567,-29.9201533172485,-29.2252829775567),
 .UNSPECIFIED.);
#1971=B_SPLINE_CURVE_WITH_KNOTS('',3,(#24571,#24572,#24573,#24574,#24575,
#24576,#24577,#24578,#24579,#24580,#24581,#24582,#24583,#24584,#24585,#24586,
#24587,#24588,#24589,#24590,#24591,#24592),.UNSPECIFIED.,.F.,.F.,(4,3,3,
3,3,3,3,4),(26.2469322667479,26.9557105598347,27.9540702101989,28.9524298605632,
29.9507895109274,30.9491491612917,31.9475088116559,32.5301175739275),
 .UNSPECIFIED.);
#1972=B_SPLINE_CURVE_WITH_KNOTS('',3,(#24597,#24598,#24599,#24600,#24601,
#24602,#24603,#24604,#24605,#24606,#24607,#24608,#24609,#24610,#24611,#24612,
#24613,#24614,#24615,#24616,#24617,#24618),.UNSPECIFIED.,.F.,.F.,(4,3,3,
3,3,3,3,4),(-41.7916535919158,-40.8908762002396,-39.8935377563313,-38.896199312423,
-37.8988608685147,-36.9015224246064,-35.9041839806982,-35.5084682847363),
 .UNSPECIFIED.);
#1973=B_SPLINE_CURVE_WITH_KNOTS('',3,(#24619,#24620,#24621,#24622,#24623,
#24624,#24625,#24626,#24627,#24628,#24629,#24630,#24631,#24632,#24633,#24634,
#24635,#24636,#24637,#24638,#24639,#24640),.UNSPECIFIED.,.F.,.F.,(4,3,3,
3,3,3,3,4),(32.5301175739275,32.9458684620202,33.9442281123844,34.9425877627486,
35.9409474131129,36.9393070634771,37.9376667138414,38.8133028811071),
 .UNSPECIFIED.);
#1974=B_SPLINE_CURVE_WITH_KNOTS('',3,(#24645,#24646,#24647,#24648,#24649,
#24650,#24651,#24652,#24653,#24654,#24655,#24656,#24657,#24658,#24659,#24660,
#24661,#24662,#24663,#24664,#24665,#24666,#24667,#24668,#24669),
 .UNSPECIFIED.,.F.,.F.,(4,3,3,3,3,3,3,3,4),(-48.0748388990954,-47.8722453075976,
-46.8749068636893,-45.877568419781,-44.8802299758727,-43.8828915319644,
-42.8855530880561,-41.8882146441479,-41.7916535919158),.UNSPECIFIED.);
#1975=B_SPLINE_CURVE_WITH_KNOTS('',3,(#24670,#24671,#24672,#24673,#24674,
#24675,#24676,#24677,#24678,#24679,#24680,#24681,#24682,#24683,#24684,#24685,
#24686,#24687,#24688,#24689,#24690,#24691,#24692,#24693,#24694),
 .UNSPECIFIED.,.F.,.F.,(4,3,3,3,3,3,3,3,4),(38.8133028811071,38.9360263642056,
39.9343860145699,40.9327456649341,41.9311053152984,42.9294649656626,43.9278246160269,
44.9261842663911,45.0964881882867),.UNSPECIFIED.);
#1976=B_SPLINE_CURVE_WITH_KNOTS('',3,(#24699,#24700,#24701,#24702,#24703,
#24704,#24705,#24706,#24707,#24708,#24709,#24710,#24711,#24712,#24713,#24714,
#24715,#24716,#24717,#24718,#24719,#24720),.UNSPECIFIED.,.F.,.F.,(4,3,3,
3,3,3,3,4),(-54.358024206275,-53.8562759710472,-52.858937527139,-51.8615990832307,
-50.8642606393224,-49.8669221954141,-48.8695837515058,-48.0748388990954),
 .UNSPECIFIED.);
#1977=B_SPLINE_CURVE_WITH_KNOTS('',3,(#24721,#24722,#24723,#24724,#24725,
#24726,#24727,#24728,#24729,#24730,#24731,#24732,#24733,#24734,#24735,#24736,
#24737,#24738,#24739,#24740,#24741,#24742),.UNSPECIFIED.,.F.,.F.,(4,3,3,
3,3,3,3,4),(45.0964881882867,45.9245439167554,46.9229035671196,47.9212632174839,
48.9196228678481,49.9179825182124,50.9163421685766,51.3796734954663),
 .UNSPECIFIED.);
#1978=B_SPLINE_CURVE_WITH_KNOTS('',3,(#24747,#24748,#24749,#24750,#24751,
#24752,#24753,#24754,#24755,#24756,#24757,#24758,#24759,#24760,#24761,#24762,
#24763,#24764,#24765,#24766,#24767,#24768),.UNSPECIFIED.,.F.,.F.,(4,3,3,
3,3,3,3,4),(-60.6412095134546,-59.8403066344969,-58.8429681905886,-57.8456297466804,
-56.8482913027721,-55.8509528588638,-54.8536144149555,-54.358024206275),
 .UNSPECIFIED.);
#1979=B_SPLINE_CURVE_WITH_KNOTS('',3,(#24769,#24770,#24771,#24772,#24773,
#24774,#24775,#24776,#24777,#24778,#24779,#24780,#24781,#24782,#24783,#24784,
#24785,#24786,#24787,#24788,#24789,#24790),.UNSPECIFIED.,.F.,.F.,(4,3,3,
3,3,3,3,4),(51.3796734954663,51.9147018189409,52.9130614693051,53.9114211196693,
54.9097807700336,55.9081404203978,56.9065000707621,57.6628588026459),
 .UNSPECIFIED.);
#1980=B_SPLINE_CURVE_WITH_KNOTS('',3,(#24796,#24797,#24798,#24799,#24800,
#24801,#24802,#24803,#24804,#24805),.UNSPECIFIED.,.F.,.F.,(4,1,1,1,1,1,
1,4),(72.2566310325653,72.4530665975158,73.4504050414241,74.4477434853324,
75.4450819292407,76.4424203731489,77.4397588170572,78.4370972609655),
 .UNSPECIFIED.);
#1981=B_SPLINE_CURVE_WITH_KNOTS('',3,(#24808,#24809,#24810,#24811,#24812,
#24813,#24814,#24815),.UNSPECIFIED.,.F.,.F.,(4,1,1,1,1,4),(72.2566310325652,
73.2039641964158,74.2023238467801,75.2006834971443,76.1990431475085,77.1974027978728),
 .UNSPECIFIED.);
#1982=B_SPLINE_CURVE_WITH_KNOTS('',3,(#24820,#24821,#24822,#24823,#24824,
#24825,#24826,#24827,#24828,#24829),.UNSPECIFIED.,.F.,.F.,(4,1,1,1,1,1,
1,4),(65.9734457253856,66.4690359340661,67.4663743779744,68.4637128218827,
69.461051265791,70.4583897096992,71.4557281536075,72.2566310325653),
 .UNSPECIFIED.);
#1983=B_SPLINE_CURVE_WITH_KNOTS('',3,(#24830,#24831,#24832,#24833,#24834,
#24835,#24836,#24837,#24838,#24839,#24840),.UNSPECIFIED.,.F.,.F.,(4,1,1,
1,1,1,1,1,4),(65.9734457253856,66.2154466438661,67.2138062942303,68.2121659445946,
69.2105255949588,70.2088852453231,71.2072448956873,72.2056045460516,72.2566310325652),
 .UNSPECIFIED.);
#1984=B_SPLINE_CURVE_WITH_KNOTS('',3,(#24845,#24846,#24847,#24848,#24849,
#24850,#24851,#24852,#24853,#24854),.UNSPECIFIED.,.F.,.F.,(4,1,1,1,1,1,
1,4),(59.6902604182061,60.4850052706164,61.4823437145247,62.479682158433,
63.4770206023413,64.4743590462496,65.4716974901578,65.9734457253856),
 .UNSPECIFIED.);
#1985=B_SPLINE_CURVE_WITH_KNOTS('',3,(#24855,#24856,#24857,#24858,#24859,
#24860,#24861,#24862,#24863,#24864),.UNSPECIFIED.,.F.,.F.,(4,1,1,1,1,1,
1,4),(59.6902604182061,60.2252887416806,61.2236483920448,62.2220080424091,
63.2203676927733,64.2187273431376,65.2170869935018,65.9734457253856),
 .UNSPECIFIED.);
#1986=B_SPLINE_CURVE_WITH_KNOTS('',3,(#24869,#24870,#24871,#24872,#24873,
#24874,#24875,#24876,#24877,#24878,#24879),.UNSPECIFIED.,.F.,.F.,(4,1,1,
1,1,1,1,1,4),(53.4070751110265,53.5036361632585,54.5009746071667,55.498313051075,
56.4956514949833,57.4929899388916,58.4903283827999,59.4876668267081,59.6902604182061),
 .UNSPECIFIED.);
#1987=B_SPLINE_CURVE_WITH_KNOTS('',3,(#24880,#24881,#24882,#24883,#24884,
#24885,#24886,#24887,#24888,#24889),.UNSPECIFIED.,.F.,.F.,(4,1,1,1,1,1,
1,4),(53.4070751110265,54.2351308394951,55.2334904898594,56.2318501402236,
57.2302097905879,58.2285694409521,59.2269290913164,59.6902604182061),
 .UNSPECIFIED.);
#1988=B_SPLINE_CURVE_WITH_KNOTS('',3,(#24894,#24895,#24896,#24897,#24898,
#24899,#24900,#24901,#24902,#24903),.UNSPECIFIED.,.F.,.F.,(4,1,1,1,1,1,
1,4),(47.1238898038469,47.5196054998088,48.516943943717,49.5142823876253,
50.5116208315336,51.5089592754419,52.5062977193502,53.4070751110265),
 .UNSPECIFIED.);
#1989=B_SPLINE_CURVE_WITH_KNOTS('',3,(#24904,#24905,#24906,#24907,#24908,
#24909,#24910,#24911,#24912,#24913,#24914),.UNSPECIFIED.,.F.,.F.,(4,1,1,
1,1,1,1,1,4),(47.1238898038469,47.2466132869454,48.2449729373096,49.2433325876739,
50.2416922380381,51.2400518884024,52.2384115387666,53.2367711891309,53.4070751110265),
 .UNSPECIFIED.);
#1990=B_SPLINE_CURVE_WITH_KNOTS('',3,(#24919,#24920,#24921,#24922,#24923,
#24924,#24925,#24926,#24927,#24928),.UNSPECIFIED.,.F.,.F.,(4,1,1,1,1,1,
1,4),(40.8407044966673,41.5355748363591,42.5329132802674,43.5302517241756,
44.5275901680839,45.5249286119922,46.5222670559005,47.1238898038469),
 .UNSPECIFIED.);
#1991=B_SPLINE_CURVE_WITH_KNOTS('',3,(#24929,#24930,#24931,#24932,#24933,
#24934,#24935,#24936,#24937,#24938),.UNSPECIFIED.,.F.,.F.,(4,1,1,1,1,1,
1,4),(40.8407044966673,41.2564553847599,42.2548150351241,43.2531746854884,
44.2515343358526,45.2498939862169,46.2482536365811,47.1238898038469),
 .UNSPECIFIED.);
#1992=B_SPLINE_CURVE_WITH_KNOTS('',3,(#24943,#24944,#24945,#24946,#24947,
#24948,#24949,#24950,#24951,#24952),.UNSPECIFIED.,.F.,.F.,(4,1,1,1,1,1,
1,4),(34.5575191894877,35.5515441729094,36.5488826168177,37.5462210607259,
38.5435595046342,39.5408979485425,40.5382363924508,40.8407044966673),
 .UNSPECIFIED.);
#1993=B_SPLINE_CURVE_WITH_KNOTS('',3,(#24953,#24954,#24955,#24956,#24957,
#24958,#24959,#24960,#24961,#24962),.UNSPECIFIED.,.F.,.F.,(4,1,1,1,1,1,
1,4),(34.5575191894877,35.2662974825744,36.2646571329387,37.2630167833029,
38.2613764336672,39.2597360840314,40.2580957343957,40.8407044966673),
 .UNSPECIFIED.);
#1994=B_SPLINE_CURVE_WITH_KNOTS('',3,(#24967,#24968,#24969,#24970,#24971,
#24972,#24973,#24974,#24975,#24976,#24977),.UNSPECIFIED.,.F.,.F.,(4,1,1,
1,1,1,1,1,4),(28.2743338823081,28.5701750655514,29.5675135094597,30.564851953368,
31.5621903972762,32.5595288411845,33.5568672850928,34.5542057290011,34.5575191894877),
 .UNSPECIFIED.);
#1995=B_SPLINE_CURVE_WITH_KNOTS('',3,(#24978,#24979,#24980,#24981,#24982,
#24983,#24984,#24985,#24986,#24987,#24988),.UNSPECIFIED.,.F.,.F.,(4,1,1,
1,1,1,1,1,4),(28.2743338823081,28.2777799300247,29.2761395803889,30.2744992307532,
31.2728588811174,32.2712185314817,33.2695781818459,34.2679378322102,34.5575191894877),
 .UNSPECIFIED.);
#1996=B_SPLINE_CURVE_WITH_KNOTS('',3,(#24993,#24994,#24995,#24996,#24997,
#24998,#24999,#25000,#25001,#25002),.UNSPECIFIED.,.F.,.F.,(4,1,1,1,1,1,
1,4),(21.9911485751285,22.5861444021017,23.58348284601,24.5808212899183,
25.5781597338266,26.5754981777348,27.5728366216431,28.2743338823081),
 .UNSPECIFIED.);
#1997=B_SPLINE_CURVE_WITH_KNOTS('',3,(#25003,#25004,#25005,#25006,#25007,
#25008,#25009,#25010,#25011,#25012),.UNSPECIFIED.,.F.,.F.,(4,1,1,1,1,1,
1,4),(21.9911485751285,22.2876220278392,23.2859816782034,24.2843413285677,
25.2827009789319,26.2810606292962,27.2794202796604,28.2743338823081),
 .UNSPECIFIED.);
#1998=B_SPLINE_CURVE_WITH_KNOTS('',3,(#25017,#25018,#25019,#25020,#25021,
#25022,#25023,#25024,#25025,#25026),.UNSPECIFIED.,.F.,.F.,(4,1,1,1,1,1,
1,4),(15.7079632679489,16.602113738652,17.5994521825603,18.5967906264686,
19.5941290703769,20.5914675142851,21.5888059581934,21.9911485751285),
 .UNSPECIFIED.);
#1999=B_SPLINE_CURVE_WITH_KNOTS('',3,(#25027,#25028,#25029,#25030,#25031,
#25032,#25033,#25034,#25035,#25036),.UNSPECIFIED.,.F.,.F.,(4,1,1,1,1,1,
1,4),(15.7079632679489,16.2974641256537,17.295823776018,18.2941834263822,
19.2925430767465,20.2909027271107,21.289262377475,21.9911485751285),
 .UNSPECIFIED.);
#2000=B_SPLINE_CURVE_WITH_KNOTS('',3,(#25039,#25040,#25041,#25042,#25043,
#25044,#25045,#25046,#25047,#25048,#25049,#25050,#25051,#25052,#25053,#25054,
#25055,#25056,#25057,#25058,#25059,#25060,#25061,#25062,#25063,#25064,#25065,
#25066,#25067,#25068,#25069,#25070,#25071,#25072,#25073,#25074,#25075,#25076,
#25077,#25078,#25079,#25080,#25081,#25082,#25083,#25084,#25085,#25086,#25087,
#25088,#25089,#25090,#25091,#25092,#25093,#25094,#25095,#25096,#25097,#25098,
#25099,#25100,#25101,#25102,#25103,#25104,#25105,#25106,#25107,#25108,#25109,
#25110,#25111,#25112,#25113,#25114,#25115,#25116,#25117,#25118,#25119,#25120,
#25121,#25122,#25123,#25124,#25125,#25126,#25127,#25128,#25129,#25130,#25131,
#25132,#25133,#25134,#25135,#25136,#25137,#25138,#25139,#25140,#25141,#25142,
#25143,#25144,#25145,#25146,#25147,#25148,#25149,#25150,#25151,#25152,#25153,
#25154,#25155,#25156,#25157,#25158,#25159,#25160,#25161,#25162,#25163,#25164,
#25165,#25166,#25167,#25168,#25169,#25170,#25171,#25172,#25173,#25174,#25175,
#25176,#25177,#25178,#25179,#25180,#25181,#25182,#25183,#25184,#25185,#25186,
#25187,#25188,#25189,#25190,#25191,#25192,#25193,#25194,#25195,#25196,#25197,
#25198,#25199,#25200,#25201,#25202,#25203,#25204,#25205,#25206,#25207,#25208,
#25209,#25210,#25211,#25212,#25213,#25214,#25215,#25216,#25217,#25218,#25219,
#25220,#25221,#25222,#25223,#25224,#25225,#25226,#25227,#25228,#25229,#25230,
#25231,#25232,#25233,#25234,#25235,#25236,#25237,#25238,#25239,#25240,#25241,
#25242,#25243),.UNSPECIFIED.,.F.,.F.,(4,3,3,3,3,3,3,3,3,3,3,3,3,3,3,3,3,
3,3,3,3,3,3,3,3,3,3,3,3,3,3,3,3,3,3,3,3,3,3,3,3,3,3,3,3,3,3,3,3,3,3,3,3,
3,3,3,3,3,3,3,3,3,3,3,3,3,3,3,4),(-0.996917990983889,-0.978871820698626,
-0.961104366684017,-0.951552920986235,-0.947856438601261,-0.928927311919591,
-0.909844934708151,-0.904827747876617,-0.901690020918146,-0.882383426909664,
-0.863197144412726,-0.849964666497242,-0.841946217765742,-0.838653066670214,
-0.836732188581758,-0.818195847210497,-0.79884286378821,-0.782668226932182,
-0.778162385717433,-0.774287931072979,-0.754720517493441,-0.734912656248282,
-0.718545934421209,-0.712508687338266,-0.709097549624951,-0.689177599037007,
-0.66944576893999,-0.649768871196005,-0.645300371314176,-0.641533261094732,
-0.621745212512907,-0.601563770435519,-0.588280416256018,-0.579851467607475,
-0.575105400436484,-0.55460765219522,-0.534203727151442,-0.514750332075477,
-0.510181591792683,-0.506682086087755,-0.495296936999511,-0.475415657124971,
-0.455258237398922,-0.446439366268775,-0.440745412953617,-0.437134753004049,
-0.41645257608894,-0.395479514073081,-0.375148710383956,-0.368821709024976,
-0.365366889657485,-0.344172462410384,-0.323356461419818,-0.31415629931658,
-0.303019600034791,-0.297245219492413,-0.293778204123757,-0.272935156968737,
-0.251638706464901,-0.237180007007782,-0.228159672465448,-0.224715742096491,
-0.221072456791868,-0.199410898099475,-0.17780203126093,-0.156885571034439,
-0.151911241963545,-0.148372189075213,-0.135969110807948),.UNSPECIFIED.);
#2001=B_SPLINE_CURVE_WITH_KNOTS('',3,(#25245,#25246,#25247,#25248,#25249,
#25250,#25251,#25252,#25253,#25254,#25255,#25256,#25257,#25258,#25259,#25260,
#25261,#25262,#25263,#25264,#25265,#25266,#25267,#25268,#25269,#25270,#25271,
#25272,#25273,#25274,#25275,#25276,#25277,#25278,#25279,#25280,#25281,#25282,
#25283,#25284,#25285,#25286,#25287,#25288,#25289,#25290,#25291,#25292,#25293,
#25294,#25295,#25296,#25297,#25298,#25299,#25300,#25301,#25302),
 .UNSPECIFIED.,.F.,.F.,(4,3,3,3,3,3,3,3,3,3,3,3,3,3,3,3,3,3,3,4),(-0.271362855059846,
-0.249815149227379,-0.228817911637578,-0.214757147690894,-0.202696405081427,
-0.199258885355278,-0.179079500439592,-0.172574855850844,-0.151002998869488,
-0.132127624010802,-0.128545226638174,-0.108660379749781,-0.0889046558653028,
-0.0695674270863146,-0.0643977980835871,-0.0611874131352371,-0.042433397437552,
-0.0240016538661123,-0.00610725636958426,0.),.UNSPECIFIED.);
#2002=B_SPLINE_CURVE_WITH_KNOTS('',3,(#25305,#25306,#25307,#25308,#25309,
#25310,#25311,#25312,#25313,#25314,#25315,#25316,#25317,#25318,#25319,#25320,
#25321,#25322,#25323,#25324,#25325,#25326,#25327,#25328,#25329,#25330,#25331,
#25332),.UNSPECIFIED.,.F.,.F.,(4,3,3,3,3,3,3,3,3,4),(-0.135969110807948,
-0.126188073854222,-0.104892740575823,-0.0831670570417323,-0.0779384685470277,
-0.0734086019617295,-0.0516285578143609,-0.0295399653803274,-0.00752416693119264,
0.),.UNSPECIFIED.);
#2003=B_SPLINE_CURVE_WITH_KNOTS('',3,(#25617,#25618,#25619,#25620,#25621,
#25622,#25623,#25624),.UNSPECIFIED.,.F.,.F.,(4,1,1,1,1,4),(11.6154215191106,
12.6127599630189,13.6100984069272,14.6074368508354,15.6047752947437,15.7079632679489),
 .UNSPECIFIED.);
#2004=B_SPLINE_CURVE_WITH_KNOTS('',3,(#25625,#25626,#25627,#25628,#25629,
#25630,#25631,#25632,#25633,#25634,#25635,#25636,#25637,#25638,#25639,#25640,
#25641,#25642,#25643,#25644,#25645,#25646,#25647,#25648,#25649,#25650,#25651,
#25652,#25653,#25654,#25655,#25656,#25657,#25658,#25659,#25660,#25661,#25662,
#25663,#25664,#25665,#25666,#25667,#25668,#25669,#25670,#25671,#25672,#25673,
#25674,#25675,#25676,#25677,#25678,#25679,#25680,#25681,#25682,#25683,#25684,
#25685,#25686,#25687,#25688,#25689,#25690,#25691,#25692,#25693,#25694,#25695,
#25696,#25697,#25698,#25699,#25700,#25701,#25702,#25703,#25704,#25705,#25706,
#25707,#25708,#25709),.UNSPECIFIED.,.F.,.F.,(4,3,3,3,3,3,3,3,3,3,3,3,3,
3,3,3,3,3,3,3,3,3,3,3,3,3,3,3,4),(-0.364629307890661,-0.350886771084415,
-0.329297510939725,-0.318979842765136,-0.313748856729508,-0.309367238941102,
-0.288044972781349,-0.272811108278258,-0.264009728102714,-0.260298972601032,
-0.239567880035138,-0.219347617431434,-0.206054227262732,-0.194878207820902,
-0.191399429390758,-0.17181371271556,-0.166174056756627,-0.145402299662048,
-0.12670765132229,-0.123381127587156,-0.103926762733045,-0.0845494608218094,
-0.0655688723802368,-0.0621691825638593,-0.0589309125894093,-0.0403408647045067,
-0.0220852216194749,-0.00441218938162483,0.),.UNSPECIFIED.);
#2005=B_SPLINE_CURVE_WITH_KNOTS('',3,(#25710,#25711,#25712,#25713,#25714,
#25715,#25716,#25717,#25718,#25719,#25720,#25721,#25722,#25723,#25724,#25725,
#25726,#25727,#25728),.UNSPECIFIED.,.F.,.F.,(4,3,3,3,3,3,4),(-65.3098882395457,
-64.8269988540384,-63.8296604101301,-62.8323219662218,-61.8349835223135,
-60.8376450784052,-60.6412095134546),.UNSPECIFIED.);
#2006=B_SPLINE_CURVE_WITH_KNOTS('',3,(#25731,#25732,#25733,#25734,#25735,
#25736,#25737,#25738,#25739),.UNSPECIFIED.,.F.,.F.,(4,1,1,1,1,1,4),(10.3757270560179,
11.3056658738325,12.3040255241967,13.302385174561,14.3007448249252,15.2991044752895,
15.7079632679489),.UNSPECIFIED.);
#2007=B_SPLINE_CURVE_WITH_KNOTS('',3,(#26029,#26030,#26031,#26032,#26033,
#26034,#26035,#26036,#26037,#26038,#26039,#26040,#26041,#26042,#26043,#26044,
#26045,#26046,#26047,#26048,#26049,#26050),.UNSPECIFIED.,.F.,.F.,(4,3,3,
3,3,3,3,4),(57.6628588026459,57.9048597211263,58.9032193714906,59.9015790218548,
60.8999386722191,61.8982983225833,62.8966579729476,63.2447481062677),
 .UNSPECIFIED.);
#2008=B_SPLINE_CURVE_WITH_KNOTS('',3,(#26051,#26052,#26053,#26054,#26055,
#26056,#26057,#26058,#26059,#26060,#26061,#26062,#26063,#26064,#26065,#26066,
#26067,#26068,#26069,#26070,#26071,#26072,#26073,#26074,#26075,#26076,#26077,
#26078,#26079,#26080,#26081,#26082,#26083,#26084,#26085,#26086,#26087,#26088,
#26089,#26090,#26091,#26092,#26093,#26094,#26095,#26096,#26097,#26098,#26099,
#26100,#26101,#26102,#26103,#26104,#26105,#26106,#26107,#26108,#26109,#26110,
#26111,#26112,#26113,#26114,#26115,#26116,#26117,#26118,#26119,#26120,#26121,
#26122,#26123,#26124,#26125,#26126,#26127,#26128,#26129,#26130,#26131,#26132),
 .UNSPECIFIED.,.F.,.F.,(4,3,3,3,3,3,3,3,3,3,3,3,3,3,3,3,3,3,3,3,3,3,3,3,
3,3,3,4),(-0.366397579005847,-0.355573362530754,-0.337605442405704,-0.327398200425482,
-0.321620335202968,-0.30281021010297,-0.288367976755365,-0.281197910953663,
-0.277581602535663,-0.258139779174731,-0.23832225991534,-0.225559780767037,
-0.21845666374658,-0.214865898441521,-0.194435927724086,-0.187272343322128,
-0.167568574984456,-0.146399230996079,-0.142991450501546,-0.122489503287978,
-0.101565610408655,-0.0804999660718792,-0.0757146540182571,-0.0722132271210984,
-0.0505693460362938,-0.0288755213118303,-0.00764564704115539,0.),
 .UNSPECIFIED.);
#2009=B_SPLINE_CURVE_WITH_KNOTS('',3,(#26402,#26403,#26404,#26405,#26406,
#26407,#26408,#26409,#26410,#26411),.UNSPECIFIED.,.F.,.F.,(4,3,3,4),(-4.09293042013066,
-3.97832038727896,-2.98374029045922,-2.06863817490914),.UNSPECIFIED.);
#2010=B_SPLINE_CURVE_WITH_KNOTS('',3,(#26414,#26415,#26416,#26417,#26418,
#26419,#26420),.UNSPECIFIED.,.F.,.F.,(4,3,4),(0.,0.995210874448857,1.11730040836817),
 .UNSPECIFIED.);
#2011=B_SPLINE_CURVE_WITH_KNOTS('',3,(#26425,#26426,#26427,#26428,#26429,
#26430,#26431,#26432,#26433,#26434,#26435,#26436,#26437,#26438,#26439,#26440,
#26441,#26442,#26443,#26444,#26445,#26446),.UNSPECIFIED.,.F.,.F.,(4,3,3,
3,3,3,3,4),(-10.3761157273102,-9.9458009681974,-8.95122087137766,-7.95664077455792,
-6.96206067773818,-5.96748058091844,-4.9729004840987,-4.09293042013066),
 .UNSPECIFIED.);
#2012=B_SPLINE_CURVE_WITH_KNOTS('',3,(#26447,#26448,#26449,#26450,#26451,
#26452,#26453,#26454,#26455,#26456,#26457,#26458,#26459,#26460,#26461,#26462,
#26463,#26464,#26465,#26466,#26467,#26468),.UNSPECIFIED.,.F.,.F.,(4,3,3,
3,3,3,3,4),(1.11730040836817,1.99042174889772,2.98563262334659,3.98084349779545,
4.97605437224432,5.97126524669318,6.96647612114205,7.40048571554776),
 .UNSPECIFIED.);
#2013=B_SPLINE_CURVE_WITH_KNOTS('',3,(#26473,#26474,#26475,#26476,#26477,
#26478,#26479,#26480,#26481,#26482,#26483,#26484,#26485,#26486,#26487,#26488,
#26489,#26490,#26491,#26492,#26493,#26494),.UNSPECIFIED.,.F.,.F.,(4,3,3,
3,3,3,3,4),(-16.6593010344898,-15.9132815491158,-14.9187014522961,-13.9241213554764,
-12.9295412586566,-11.9349611618369,-10.9403810650171,-10.3761157273102),
 .UNSPECIFIED.);
#2014=B_SPLINE_CURVE_WITH_KNOTS('',3,(#26495,#26496,#26497,#26498,#26499,
#26500,#26501,#26502,#26503,#26504,#26505,#26506,#26507,#26508,#26509,#26510,
#26511,#26512,#26513,#26514,#26515,#26516),.UNSPECIFIED.,.F.,.F.,(4,3,3,
3,3,3,3,4),(7.40048571554776,7.96168699559091,8.95689787003978,9.95210874448864,
10.9473196189375,11.9425304933864,12.9377413678352,13.6836710227273),
 .UNSPECIFIED.);
#2015=B_SPLINE_CURVE_WITH_KNOTS('',3,(#26521,#26522,#26523,#26524,#26525,
#26526,#26527,#26528,#26529,#26530,#26531,#26532,#26533,#26534,#26535,#26536,
#26537,#26538,#26539,#26540,#26541,#26542,#26543,#26544,#26545),
 .UNSPECIFIED.,.F.,.F.,(4,3,3,3,3,3,3,3,4),(-22.9424863416694,-22.875342226854,
-21.8807621300343,-20.8861820332145,-19.8916019363948,-18.8970218395751,
-17.9024417427553,-16.9078616459356,-16.6593010344898),.UNSPECIFIED.);
#2016=B_SPLINE_CURVE_WITH_KNOTS('',3,(#26546,#26547,#26548,#26549,#26550,
#26551,#26552,#26553,#26554,#26555,#26556,#26557,#26558,#26559,#26560,#26561,
#26562,#26563,#26564,#26565,#26566,#26567,#26568,#26569,#26570),
 .UNSPECIFIED.,.F.,.F.,(4,3,3,3,3,3,3,3,4),(13.6836710227273,13.9329522422841,
14.928163116733,15.9233739911818,16.9185848656307,17.9137957400795,18.9090066145284,
19.9042174889773,19.9668563299069),.UNSPECIFIED.);
#2017=B_SPLINE_CURVE_WITH_KNOTS('',3,(#26575,#26576,#26577,#26578,#26579,
#26580,#26581,#26582,#26583,#26584,#26585,#26586,#26587,#26588,#26589,#26590,
#26591,#26592,#26593,#26594,#26595,#26596),.UNSPECIFIED.,.F.,.F.,(4,3,3,
3,3,3,3,4),(-29.225671648849,-28.8428228077724,-27.8482427109527,-26.853662614133,
-25.8590825173132,-24.8645024204935,-23.8699223236738,-22.9424863416694),
 .UNSPECIFIED.);
#2018=B_SPLINE_CURVE_WITH_KNOTS('',3,(#26597,#26598,#26599,#26600,#26601,
#26602,#26603,#26604,#26605,#26606,#26607,#26608,#26609,#26610,#26611,#26612,
#26613,#26614,#26615,#26616,#26617,#26618),.UNSPECIFIED.,.F.,.F.,(4,3,3,
3,3,3,3,4),(19.9668563299069,20.8994283634261,21.894639237875,22.8898501123239,
23.8850609867727,24.8802718612216,25.8754827356705,26.2500416370865),
 .UNSPECIFIED.);
#2019=B_SPLINE_CURVE_WITH_KNOTS('',3,(#26623,#26624,#26625,#26626,#26627,
#26628,#26629,#26630,#26631,#26632,#26633,#26634,#26635,#26636,#26637,#26638,
#26639,#26640,#26641,#26642,#26643,#26644),.UNSPECIFIED.,.F.,.F.,(4,3,3,
3,3,3,3,4),(-35.5088569560286,-34.8103033886909,-33.8157232918711,-32.8211431950514,
-31.8265630982317,-30.8319830014119,-29.8374029045922,-29.225671648849),
 .UNSPECIFIED.);
#2020=B_SPLINE_CURVE_WITH_KNOTS('',3,(#26645,#26646,#26647,#26648,#26649,
#26650,#26651,#26652,#26653,#26654,#26655,#26656,#26657,#26658,#26659,#26660,
#26661,#26662,#26663,#26664,#26665,#26666),.UNSPECIFIED.,.F.,.F.,(4,3,3,
3,3,3,3,4),(26.2500416370865,26.8706936101193,27.8659044845682,28.861115359017,
29.8563262334659,30.8515371079148,31.8467479823636,32.5332269442661),
 .UNSPECIFIED.);
#2021=B_SPLINE_CURVE_WITH_KNOTS('',3,(#26671,#26672,#26673,#26674,#26675,
#26676,#26677,#26678,#26679,#26680,#26681,#26682,#26683,#26684,#26685,#26686,
#26687,#26688,#26689,#26690,#26691,#26692,#26693,#26694,#26695),
 .UNSPECIFIED.,.F.,.F.,(4,3,3,3,3,3,3,3,4),(-41.7920422632082,-41.7723640664291,
-40.7777839696093,-39.7832038727896,-38.7886237759698,-37.7940436791501,
-36.7994635823304,-35.8048834855106,-35.5088569560286),.UNSPECIFIED.);
#2022=B_SPLINE_CURVE_WITH_KNOTS('',3,(#26696,#26697,#26698,#26699,#26700,
#26701,#26702,#26703,#26704,#26705,#26706,#26707,#26708,#26709,#26710,#26711,
#26712,#26713,#26714,#26715,#26716,#26717,#26718,#26719,#26720),
 .UNSPECIFIED.,.F.,.F.,(4,3,3,3,3,3,3,3,4),(32.5332269442661,32.8419588568125,
33.8371697312614,34.8323806057102,35.8275914801591,36.822802354608,37.8180132290568,
38.8132241035057,38.8164122514457),.UNSPECIFIED.);
#2023=B_SPLINE_CURVE_WITH_KNOTS('',3,(#26725,#26726,#26727,#26728,#26729,
#26730,#26731,#26732,#26733,#26734,#26735,#26736,#26737,#26738,#26739,#26740,
#26741,#26742,#26743,#26744,#26745,#26746),.UNSPECIFIED.,.F.,.F.,(4,3,3,
3,3,3,3,4),(-48.0752275703878,-47.7398446473475,-46.7452645505278,-45.750684453708,
-44.7561043568883,-43.7615242600685,-42.7669441632488,-41.7920422632082),
 .UNSPECIFIED.);
#2024=B_SPLINE_CURVE_WITH_KNOTS('',3,(#26747,#26748,#26749,#26750,#26751,
#26752,#26753,#26754,#26755,#26756,#26757,#26758,#26759,#26760,#26761,#26762,
#26763,#26764,#26765,#26766,#26767,#26768),.UNSPECIFIED.,.F.,.F.,(4,3,3,
3,3,3,3,4),(38.8164122514457,39.8084349779546,40.8036458524034,41.7988567268523,
42.7940676013012,43.78927847575,44.7844893501989,45.0995975586253),
 .UNSPECIFIED.);
#2025=B_SPLINE_CURVE_WITH_KNOTS('',3,(#26773,#26774,#26775,#26776,#26777,
#26778,#26779,#26780,#26781,#26782,#26783,#26784,#26785,#26786,#26787,#26788,
#26789,#26790,#26791,#26792,#26793,#26794),.UNSPECIFIED.,.F.,.F.,(4,3,3,
3,3,3,3,4),(-54.3584128775674,-53.7073252282659,-52.7127451314462,-51.7181650346265,
-50.7235849378067,-49.729004840987,-48.7344247441672,-48.0752275703878),
 .UNSPECIFIED.);
#2026=B_SPLINE_CURVE_WITH_KNOTS('',3,(#26795,#26796,#26797,#26798,#26799,
#26800,#26801,#26802,#26803,#26804,#26805,#26806,#26807,#26808,#26809,#26810,
#26811,#26812,#26813,#26814,#26815,#26816),.UNSPECIFIED.,.F.,.F.,(4,3,3,
3,3,3,3,4),(45.0995975586253,45.7797002246477,46.7749110990966,47.7701219735455,
48.7653328479943,49.7605437224432,50.7557545968921,51.3827828658049),
 .UNSPECIFIED.);
#2027=B_SPLINE_CURVE_WITH_KNOTS('',3,(#26821,#26822,#26823,#26824,#26825,
#26826,#26827,#26828,#26829,#26830,#26831,#26832,#26833,#26834,#26835,#26836,
#26837,#26838,#26839,#26840,#26841,#26842),.UNSPECIFIED.,.F.,.F.,(4,3,3,
3,3,3,3,4),(-60.641598184747,-59.6748058091844,-58.6802257123646,-57.6856456155449,
-56.6910655187252,-55.6964854219054,-54.7019053250857,-54.3584128775674),
 .UNSPECIFIED.);
#2028=B_SPLINE_CURVE_WITH_KNOTS('',3,(#26843,#26844,#26845,#26846,#26847,
#26848,#26849,#26850,#26851,#26852,#26853,#26854,#26855,#26856,#26857,#26858,
#26859,#26860,#26861,#26862,#26863,#26864),.UNSPECIFIED.,.F.,.F.,(4,3,3,
3,3,3,3,4),(51.3827828658049,51.7509654713409,52.7461763457898,53.7413872202387,
54.7365980946875,55.7318089691364,56.7270198435852,57.6659681729845),
 .UNSPECIFIED.);
#2029=B_SPLINE_CURVE_WITH_KNOTS('',3,(#26869,#26870,#26871,#26872,#26873,
#26874,#26875,#26876,#26877,#26878,#26879,#26880,#26881,#26882,#26883,#26884,
#26885,#26886,#26887,#26888,#26889,#26890,#26891,#26892,#26893),
 .UNSPECIFIED.,.F.,.F.,(4,3,3,3,3,3,3,3,4),(-66.9247834919266,-66.6368664869226,
-65.6422863901028,-64.6477062932831,-63.6531261964633,-62.6585460996436,
-61.6639660028239,-60.6693859060041,-60.641598184747),.UNSPECIFIED.);
#2030=B_SPLINE_CURVE_WITH_KNOTS('',3,(#26894,#26895,#26896,#26897,#26898,
#26899,#26900,#26901,#26902,#26903,#26904,#26905,#26906,#26907,#26908,#26909,
#26910,#26911,#26912,#26913,#26914,#26915,#26916,#26917,#26918),
 .UNSPECIFIED.,.F.,.F.,(4,3,3,3,3,3,3,3,4),(57.6659681729845,57.7222307180341,
58.717441592483,59.7126524669318,60.7078633413807,61.7030742158296,62.6982850902784,
63.6934959647273,63.9491534801641),.UNSPECIFIED.);
#2031=B_SPLINE_CURVE_WITH_KNOTS('',3,(#26923,#26924,#26925,#26926,#26927,
#26928,#26929,#26930,#26931,#26932,#26933,#26934,#26935,#26936,#26937,#26938,
#26939,#26940,#26941,#26942,#26943,#26944),.UNSPECIFIED.,.F.,.F.,(4,3,3,
3,3,3,3,4),(-73.2079687991062,-72.604347067841,-71.6097669710212,-70.6151868742015,
-69.6206067773818,-68.626026680562,-67.6314465837423,-66.9247834919266),
 .UNSPECIFIED.);
#2032=B_SPLINE_CURVE_WITH_KNOTS('',3,(#26945,#26946,#26947,#26948,#26949,
#26950,#26951,#26952,#26953,#26954,#26955,#26956,#26957,#26958,#26959,#26960,
#26961,#26962,#26963,#26964,#26965,#26966),.UNSPECIFIED.,.F.,.F.,(4,3,3,
3,3,3,3,4),(63.9491534801641,64.6887068391762,65.683917713625,66.6791285880739,
67.6743394625228,68.6695503369716,69.6647612114205,70.2323387873437),
 .UNSPECIFIED.);
#2033=B_SPLINE_CURVE_WITH_KNOTS('',3,(#26971,#26972,#26973,#26974,#26975,
#26976,#26977,#26978,#26979,#26980,#26981,#26982,#26983,#26984,#26985,#26986,
#26987,#26988,#26989,#26990,#26991,#26992),.UNSPECIFIED.,.F.,.F.,(4,3,3,
3,3,3,3,4),(-79.4911541062857,-78.5718276487594,-77.5772475519397,-76.5826674551199,
-75.5880873583002,-74.5935072614805,-73.5989271646607,-73.2079687991062),
 .UNSPECIFIED.);
#2034=B_SPLINE_CURVE_WITH_KNOTS('',3,(#26993,#26994,#26995,#26996,#26997,
#26998,#26999,#27000,#27001,#27002,#27003,#27004,#27005,#27006,#27007,#27008,
#27009,#27010,#27011,#27012,#27013,#27014),.UNSPECIFIED.,.F.,.F.,(4,3,3,
3,3,3,3,4),(70.2323387873437,70.6599720858693,71.6551829603182,72.6503938347671,
73.6456047092159,74.6408155836648,75.6360264581137,76.5155240945233),
 .UNSPECIFIED.);
#2035=B_SPLINE_CURVE_WITH_KNOTS('',3,(#27019,#27020,#27021,#27022,#27023,
#27024,#27025,#27026,#27027,#27028,#27029,#27030,#27031,#27032,#27033,#27034,
#27035,#27036,#27037,#27038,#27039,#27040,#27041,#27042,#27043),
 .UNSPECIFIED.,.F.,.F.,(4,3,3,3,3,3,3,3,4),(-85.7743394134653,-85.5338883264976,
-84.5393082296779,-83.5447281328581,-82.5501480360384,-81.5555679392187,
-80.5609878423989,-79.5664077455792,-79.4911541062857),.UNSPECIFIED.);
#2036=B_SPLINE_CURVE_WITH_KNOTS('',3,(#27044,#27045,#27046,#27047,#27048,
#27049,#27050,#27051,#27052,#27053,#27054,#27055,#27056,#27057,#27058,#27059,
#27060,#27061,#27062,#27063,#27064,#27065,#27066,#27067,#27068),
 .UNSPECIFIED.,.F.,.F.,(4,3,3,3,3,3,3,3,4),(76.5155240945233,76.6312373325625,
77.6264482070114,78.6216590814603,79.6168699559091,80.612080830358,81.6072917048068,
82.6025025792557,82.7987094017029),.UNSPECIFIED.);
#2037=B_SPLINE_CURVE_WITH_KNOTS('',3,(#27073,#27074,#27075,#27076,#27077,
#27078,#27079,#27080,#27081,#27082,#27083,#27084,#27085,#27086,#27087,#27088,
#27089,#27090,#27091,#27092,#27093,#27094),.UNSPECIFIED.,.F.,.F.,(4,3,3,
3,3,3,3,4),(-92.0575247206449,-91.501368907416,-90.5067888105963,-89.5122087137766,
-88.5176286169568,-87.5230485201371,-86.5284684233173,-85.7743394134653),
 .UNSPECIFIED.);
#2038=B_SPLINE_CURVE_WITH_KNOTS('',3,(#27095,#27096,#27097,#27098,#27099,
#27100,#27101,#27102,#27103,#27104,#27105,#27106,#27107,#27108,#27109,#27110,
#27111,#27112,#27113,#27114,#27115,#27116),.UNSPECIFIED.,.F.,.F.,(4,3,3,
3,3,3,3,4),(82.7987094017029,83.5977134537046,84.5929243281534,85.5881352026023,
86.5833460770512,87.5785569515,88.5737678259489,89.0818947088824),
 .UNSPECIFIED.);
#2039=B_SPLINE_CURVE_WITH_KNOTS('',3,(#27121,#27122,#27123,#27124,#27125,
#27126,#27127,#27128,#27129,#27130,#27131,#27132,#27133,#27134,#27135,#27136,
#27137,#27138,#27139,#27140,#27141,#27142),.UNSPECIFIED.,.F.,.F.,(4,3,3,
3,3,3,3,4),(-98.3407100278245,-97.4688494883345,-96.4742693915147,-95.479689294695,
-94.4851091978752,-93.4905291010555,-92.4959490042358,-92.0575247206449),
 .UNSPECIFIED.);
#2040=B_SPLINE_CURVE_WITH_KNOTS('',3,(#27143,#27144,#27145,#27146,#27147,
#27148,#27149,#27150,#27151,#27152,#27153,#27154,#27155,#27156,#27157,#27158,
#27159,#27160,#27161,#27162,#27163,#27164),.UNSPECIFIED.,.F.,.F.,(4,3,3,
3,3,3,3,4),(89.0818947088824,89.5689787003978,90.5641895748466,91.5594004492955,
92.5546113237443,93.5498221981932,94.5450330726421,95.365080016062),
 .UNSPECIFIED.);
#2041=B_SPLINE_CURVE_WITH_KNOTS('',3,(#27169,#27170,#27171,#27172,#27173,
#27174,#27175,#27176,#27177,#27178,#27179,#27180,#27181,#27182,#27183,#27184,
#27185,#27186,#27187,#27188,#27189,#27190,#27191,#27192,#27193),
 .UNSPECIFIED.,.F.,.F.,(4,3,3,3,3,3,3,3,4),(-104.623895335004,-104.430910166073,
-103.436330069253,-102.441749972433,-101.447169875613,-100.452589778794,
-99.458009681974,-98.4634295851542,-98.3407100278245),.UNSPECIFIED.);
#2042=B_SPLINE_CURVE_WITH_KNOTS('',3,(#27194,#27195,#27196,#27197,#27198,
#27199,#27200,#27201,#27202,#27203,#27204,#27205,#27206,#27207,#27208,#27209,
#27210,#27211,#27212,#27213,#27214,#27215,#27216,#27217,#27218),
 .UNSPECIFIED.,.F.,.F.,(4,3,3,3,3,3,3,3,4),(95.365080016062,95.5402439470909,
96.5354548215398,97.5306656959886,98.5258765704375,99.5210874448864,100.516298319335,
101.511509193784,101.648265323242),.UNSPECIFIED.);
#2043=B_SPLINE_CURVE_WITH_KNOTS('',3,(#27223,#27224,#27225,#27226,#27227,
#27228,#27229,#27230,#27231,#27232,#27233,#27234,#27235,#27236,#27237,#27238,
#27239,#27240,#27241,#27242,#27243,#27244),.UNSPECIFIED.,.F.,.F.,(4,3,3,
3,3,3,3,4),(-110.907080642184,-110.398390746991,-109.403810650171,-108.409230553352,
-107.414650456532,-106.420070359712,-105.425490262892,-104.623895335004),
 .UNSPECIFIED.);
#2044=B_SPLINE_CURVE_WITH_KNOTS('',3,(#27245,#27246,#27247,#27248,#27249,
#27250,#27251,#27252,#27253,#27254,#27255,#27256,#27257,#27258,#27259,#27260,
#27261,#27262,#27263,#27264,#27265,#27266),.UNSPECIFIED.,.F.,.F.,(4,3,3,
3,3,3,3,4),(101.648265323242,102.506720068233,103.501930942682,104.497141817131,
105.49235269158,106.487563566028,107.482774440477,107.931450630421),
 .UNSPECIFIED.);
#2045=B_SPLINE_CURVE_WITH_KNOTS('',3,(#27271,#27272,#27273,#27274,#27275,
#27276,#27277,#27278,#27279,#27280,#27281,#27282,#27283,#27284,#27285,#27286,
#27287,#27288,#27289,#27290,#27291,#27292),.UNSPECIFIED.,.F.,.F.,(4,3,3,
3,3,3,3,4),(-117.190265949363,-116.36587132791,-115.37129123109,-114.37671113427,
-113.38213103745,-112.387550940631,-111.392970843811,-110.907080642184),
 .UNSPECIFIED.);
#2046=B_SPLINE_CURVE_WITH_KNOTS('',3,(#27293,#27294,#27295,#27296,#27297,
#27298,#27299,#27300,#27301,#27302,#27303,#27304,#27305,#27306,#27307,#27308,
#27309,#27310,#27311,#27312,#27313,#27314),.UNSPECIFIED.,.F.,.F.,(4,3,3,
3,3,3,3,4),(107.931450630421,108.477985314926,109.473196189375,110.468407063824,
111.463617938273,112.458828812722,113.454039687171,114.214635937601),
 .UNSPECIFIED.);
#2047=B_SPLINE_CURVE_WITH_KNOTS('',3,(#27320,#27321,#27322,#27323,#27324,
#27325,#27326,#27327,#27328,#27329),.UNSPECIFIED.,.F.,.F.,(4,1,1,1,1,1,
1,4),(128.805298797182,128.975484272548,129.970064369367,130.964644466187,
131.959224563007,132.953804659826,133.948384756646,134.942964853466),
 .UNSPECIFIED.);
#2048=B_SPLINE_CURVE_WITH_KNOTS('',3,(#27332,#27333,#27334,#27335,#27336,
#27337,#27338,#27339),.UNSPECIFIED.,.F.,.F.,(4,1,1,1,1,4),(128.805298797182,
129.723204235162,130.718415109611,131.71362598406,132.708836858509,133.704047732958),
 .UNSPECIFIED.);
#2049=B_SPLINE_CURVE_WITH_KNOTS('',3,(#27344,#27345,#27346,#27347,#27348,
#27349,#27350,#27351,#27352,#27353),.UNSPECIFIED.,.F.,.F.,(4,1,1,1,1,1,
1,4),(122.522113490002,123.008003691629,124.002583788449,124.997163885269,
125.991743982088,126.986324078908,127.980904175728,128.805298797182),
 .UNSPECIFIED.);
#2050=B_SPLINE_CURVE_WITH_KNOTS('',3,(#27354,#27355,#27356,#27357,#27358,
#27359,#27360,#27361,#27362,#27363,#27364),.UNSPECIFIED.,.F.,.F.,(4,1,1,
1,1,1,1,1,4),(122.522113490002,122.75672811402,123.751938988469,124.747149862918,
125.742360737367,126.737571611816,127.732782486265,128.727993360714,128.805298797182),
 .UNSPECIFIED.);
#2051=B_SPLINE_CURVE_WITH_KNOTS('',3,(#27369,#27370,#27371,#27372,#27373,
#27374,#27375,#27376,#27377,#27378),.UNSPECIFIED.,.F.,.F.,(4,1,1,1,1,1,
1,4),(116.238928182822,117.040523110711,118.03510320753,119.02968330435,
120.02426340117,121.01884349799,122.013423594809,122.522113490002),
 .UNSPECIFIED.);
#2052=B_SPLINE_CURVE_WITH_KNOTS('',3,(#27379,#27380,#27381,#27382,#27383,
#27384,#27385,#27386,#27387,#27388),.UNSPECIFIED.,.F.,.F.,(4,1,1,1,1,1,
1,4),(116.238928182822,116.785462867327,117.780673741776,118.775884616225,
119.771095490674,120.766306365123,121.761517239572,122.522113490002),
 .UNSPECIFIED.);
#2053=B_SPLINE_CURVE_WITH_KNOTS('',3,(#27393,#27394,#27395,#27396,#27397,
#27398,#27399,#27400,#27401,#27402,#27403),.UNSPECIFIED.,.F.,.F.,(4,1,1,
1,1,1,1,1,4),(109.955742875643,110.078462432972,111.073042529792,112.067622626612,
113.062202723432,114.056782820251,115.051362917071,116.045943013891,116.238928182822),
 .UNSPECIFIED.);
#2054=B_SPLINE_CURVE_WITH_KNOTS('',3,(#27404,#27405,#27406,#27407,#27408,
#27409,#27410,#27411,#27412,#27413),.UNSPECIFIED.,.F.,.F.,(4,1,1,1,1,1,
1,4),(109.955742875643,110.814197620634,111.809408495083,112.804619369532,
113.799830243981,114.795041118429,115.790251992878,116.238928182822),
 .UNSPECIFIED.);
#2055=B_SPLINE_CURVE_WITH_KNOTS('',3,(#27418,#27419,#27420,#27421,#27422,
#27423,#27424,#27425,#27426,#27427),.UNSPECIFIED.,.F.,.F.,(4,1,1,1,1,1,
1,4),(103.672557568463,104.110981852054,105.105561948874,106.100142045694,
107.094722142513,108.089302239333,109.083882336153,109.955742875643),
 .UNSPECIFIED.);
#2056=B_SPLINE_CURVE_WITH_KNOTS('',3,(#27428,#27429,#27430,#27431,#27432,
#27433,#27434,#27435,#27436,#27437,#27438),.UNSPECIFIED.,.F.,.F.,(4,1,1,
1,1,1,1,1,4),(103.672557568463,103.847721499492,104.842932373941,105.83814324839,
106.833354122839,107.828564997287,108.823775871736,109.818986746185,109.955742875643),
 .UNSPECIFIED.);
#2057=B_SPLINE_CURVE_WITH_KNOTS('',3,(#27443,#27444,#27445,#27446,#27447,
#27448,#27449,#27450,#27451,#27452),.UNSPECIFIED.,.F.,.F.,(4,1,1,1,1,1,
1,4),(97.3893722612836,98.1435012711356,99.1380813679553,100.132661464775,
101.127241561595,102.121821658415,103.116401755234,103.672557568463),
 .UNSPECIFIED.);
#2058=B_SPLINE_CURVE_WITH_KNOTS('',3,(#27453,#27454,#27455,#27456,#27457,
#27458,#27459,#27460,#27461,#27462),.UNSPECIFIED.,.F.,.F.,(4,1,1,1,1,1,
1,4),(97.3893722612836,97.8764562527988,98.8716671272477,99.8668780016965,
100.862088876145,101.857299750594,102.852510625043,103.672557568463),
 .UNSPECIFIED.);
#2059=B_SPLINE_CURVE_WITH_KNOTS('',3,(#27467,#27468,#27469,#27470,#27471,
#27472,#27473,#27474,#27475,#27476,#27477),.UNSPECIFIED.,.F.,.F.,(4,1,1,
1,1,1,1,1,4),(91.106186954104,91.1814405933974,92.1760206902171,93.1706007870369,
94.1651808838566,95.1597609806764,96.1543410774961,97.1489211743159,97.3893722612836),
 .UNSPECIFIED.);
#2060=B_SPLINE_CURVE_WITH_KNOTS('',3,(#27478,#27479,#27480,#27481,#27482,
#27483,#27484,#27485,#27486,#27487),.UNSPECIFIED.,.F.,.F.,(4,1,1,1,1,1,
1,4),(91.106186954104,91.9051910061056,92.9004018805545,93.8956127550033,
94.8908236294522,95.8860345039011,96.8812453783499,97.3893722612836),
 .UNSPECIFIED.);
#2061=B_SPLINE_CURVE_WITH_KNOTS('',3,(#27492,#27493,#27494,#27495,#27496,
#27497,#27498,#27499,#27500,#27501),.UNSPECIFIED.,.F.,.F.,(4,1,1,1,1,1,
1,4),(84.8230016469244,85.213960012479,86.2085401092987,87.2031202061185,
88.1977003029382,89.1922803997579,90.1868604965777,91.106186954104),
 .UNSPECIFIED.);
#2062=B_SPLINE_CURVE_WITH_KNOTS('',3,(#27502,#27503,#27504,#27505,#27506,
#27507,#27508,#27509,#27510,#27511,#27512),.UNSPECIFIED.,.F.,.F.,(4,1,1,
1,1,1,1,1,4),(84.8230016469244,84.9387148849636,85.9339257594124,86.9291366338613,
87.9243475083101,88.919558382759,89.9147692572079,90.9099801316567,91.106186954104),
 .UNSPECIFIED.);
#2063=B_SPLINE_CURVE_WITH_KNOTS('',3,(#27517,#27518,#27519,#27520,#27521,
#27522,#27523,#27524,#27525,#27526),.UNSPECIFIED.,.F.,.F.,(4,1,1,1,1,1,
1,4),(78.5398163397448,79.2464794315605,80.2410595283803,81.2356396252,
82.2302197220198,83.2247998188395,84.2193799156592,84.8230016469244),
 .UNSPECIFIED.);
#2064=B_SPLINE_CURVE_WITH_KNOTS('',3,(#27527,#27528,#27529,#27530,#27531,
#27532,#27533,#27534,#27535,#27536),.UNSPECIFIED.,.F.,.F.,(4,1,1,1,1,1,
1,4),(78.5398163397448,78.9674496382704,79.9626605127192,80.9578713871681,
81.953082261617,82.9482931360658,83.9435040105147,84.8230016469244),
 .UNSPECIFIED.);
#2065=B_SPLINE_CURVE_WITH_KNOTS('',3,(#27541,#27542,#27543,#27544,#27545,
#27546,#27547,#27548,#27549,#27550,#27551),.UNSPECIFIED.,.F.,.F.,(4,1,1,
1,1,1,1,1,4),(72.2566310325652,72.2844187538224,73.2789988506421,74.2735789474618,
75.2681590442816,76.2627391411013,77.2573192379211,78.2518993347408,78.5398163397448),
 .UNSPECIFIED.);
#2066=B_SPLINE_CURVE_WITH_KNOTS('',3,(#27552,#27553,#27554,#27555,#27556,
#27557,#27558,#27559,#27560,#27561),.UNSPECIFIED.,.F.,.F.,(4,1,1,1,1,1,
1,4),(72.2566310325652,72.9961843915772,73.9913952660261,74.9866061404749,
75.9818170149238,76.9770278893726,77.9722387638215,78.5398163397448),
 .UNSPECIFIED.);
#2067=B_SPLINE_CURVE_WITH_KNOTS('',3,(#27566,#27567,#27568,#27569,#27570,
#27571,#27572,#27573,#27574,#27575),.UNSPECIFIED.,.F.,.F.,(4,1,1,1,1,1,
1,4),(65.9734457253856,66.3169381729039,67.3115182697237,68.3060983665434,
69.3006784633631,70.2952585601829,71.2898386570026,72.2566310325652),
 .UNSPECIFIED.);
#2068=B_SPLINE_CURVE_WITH_KNOTS('',3,(#27576,#27577,#27578,#27579,#27580,
#27581,#27582,#27583,#27584,#27585,#27586),.UNSPECIFIED.,.F.,.F.,(4,1,1,
1,1,1,1,1,4),(65.9734457253856,66.0297082704352,67.024919144884,68.0201300193329,
69.0153408937817,70.0105517682306,71.0057626426795,72.0009735171283,72.2566310325652),
 .UNSPECIFIED.);
#2069=B_SPLINE_CURVE_WITH_KNOTS('',3,(#27591,#27592,#27593,#27594,#27595,
#27596,#27597,#27598,#27599,#27600),.UNSPECIFIED.,.F.,.F.,(4,1,1,1,1,1,
1,4),(59.690260418206,60.3494575919855,61.3440376888052,62.338617785625,
63.3331978824447,64.3277779792645,65.3223580760842,65.9734457253856),
 .UNSPECIFIED.);
#2070=B_SPLINE_CURVE_WITH_KNOTS('',3,(#27601,#27602,#27603,#27604,#27605,
#27606,#27607,#27608,#27609,#27610),.UNSPECIFIED.,.F.,.F.,(4,1,1,1,1,1,
1,4),(59.690260418206,60.058443023742,61.0536538981908,62.0488647726397,
63.0440756470886,64.0392865215374,65.0344973959863,65.9734457253856),
 .UNSPECIFIED.);
#2071=B_SPLINE_CURVE_WITH_KNOTS('',3,(#27615,#27616,#27617,#27618,#27619,
#27620,#27621,#27622,#27623,#27624),.UNSPECIFIED.,.F.,.F.,(4,1,1,1,1,1,
1,4),(53.4070751110264,54.3819770110671,55.3765571078868,56.3711372047065,
57.3657173015263,58.360297398346,59.3548774951657,59.690260418206),
 .UNSPECIFIED.);
#2072=B_SPLINE_CURVE_WITH_KNOTS('',3,(#27625,#27626,#27627,#27628,#27629,
#27630,#27631,#27632,#27633,#27634),.UNSPECIFIED.,.F.,.F.,(4,1,1,1,1,1,
1,4),(53.4070751110264,54.0871777770488,55.0823886514976,56.0775995259465,
57.0728104003954,58.0680212748442,59.0632321492931,59.690260418206),
 .UNSPECIFIED.);
#2073=B_SPLINE_CURVE_WITH_KNOTS('',3,(#27639,#27640,#27641,#27642,#27643,
#27644,#27645,#27646,#27647,#27648,#27649),.UNSPECIFIED.,.F.,.F.,(4,1,1,
1,1,1,1,1,4),(47.1238898038468,47.4199163333289,48.4144964301486,49.4090765269684,
50.4036566237881,51.3982367206078,52.3928168174276,53.3873969142473,53.4070751110264),
 .UNSPECIFIED.);
#2074=B_SPLINE_CURVE_WITH_KNOTS('',3,(#27650,#27651,#27652,#27653,#27654,
#27655,#27656,#27657,#27658,#27659),.UNSPECIFIED.,.F.,.F.,(4,1,1,1,1,1,
1,4),(47.1238898038468,48.1159125303556,49.1111234048045,50.1063342792533,
51.1015451537022,52.096756028151,53.0919669025999,53.4070751110264),
 .UNSPECIFIED.);
#2075=B_SPLINE_CURVE_WITH_KNOTS('',3,(#27664,#27665,#27666,#27667,#27668,
#27669,#27670,#27671,#27672,#27673),.UNSPECIFIED.,.F.,.F.,(4,1,1,1,1,1,
1,4),(40.8407044966673,41.4524357524104,42.4470158492302,43.4415959460499,
44.4361760428697,45.4307561396894,46.4253362365091,47.1238898038468),
 .UNSPECIFIED.);
#2076=B_SPLINE_CURVE_WITH_KNOTS('',3,(#27674,#27675,#27676,#27677,#27678,
#27679,#27680,#27681,#27682,#27683,#27684),.UNSPECIFIED.,.F.,.F.,(4,1,1,
1,1,1,1,1,4),(40.8407044966672,41.1494364092135,42.1446472836624,43.1398581581113,
44.1350690325601,45.130279907009,46.1254907814579,47.1207016559067,47.1238898038468),
 .UNSPECIFIED.);
#2077=B_SPLINE_CURVE_WITH_KNOTS('',3,(#27689,#27690,#27691,#27692,#27693,
#27694,#27695,#27696,#27697,#27698),.UNSPECIFIED.,.F.,.F.,(4,1,1,1,1,1,
1,4),(34.5575191894877,35.484955171492,36.4795352683117,37.4741153651315,
38.4686954619512,39.463275558771,40.4578556555907,40.8407044966673),
 .UNSPECIFIED.);
#2078=B_SPLINE_CURVE_WITH_KNOTS('',3,(#27699,#27700,#27701,#27702,#27703,
#27704,#27705,#27706,#27707,#27708),.UNSPECIFIED.,.F.,.F.,(4,1,1,1,1,1,
1,4),(34.5575191894876,35.1781711625204,36.1733820369692,37.1685929114181,
38.163803785867,39.1590146603158,40.1542255347647,40.8407044966672),
 .UNSPECIFIED.);
#2079=B_SPLINE_CURVE_WITH_KNOTS('',3,(#27713,#27714,#27715,#27716,#27717,
#27718,#27719,#27720,#27721,#27722,#27723),.UNSPECIFIED.,.F.,.F.,(4,1,1,
1,1,1,1,1,4),(28.2743338823081,28.5228944937538,29.5174745905736,30.5120546873933,
31.506634784213,32.5012148810328,33.4957949778525,34.4903750746723,34.5575191894877),
 .UNSPECIFIED.);
#2080=B_SPLINE_CURVE_WITH_KNOTS('',3,(#27724,#27725,#27726,#27727,#27728,
#27729,#27730,#27731,#27732,#27733),.UNSPECIFIED.,.F.,.F.,(4,1,1,1,1,1,
1,4),(28.274333882308,29.2069059158272,30.202116790276,31.1973276647249,
32.1925385391738,33.1877494136226,34.1829602880715,34.5575191894876),
 .UNSPECIFIED.);
#2081=B_SPLINE_CURVE_WITH_KNOTS('',3,(#27738,#27739,#27740,#27741,#27742,
#27743,#27744,#27745,#27746,#27747),.UNSPECIFIED.,.F.,.F.,(4,1,1,1,1,1,
1,4),(21.9911485751285,22.5554139128354,23.5499940096551,24.5445741064749,
25.5391542032946,26.5337343001143,27.5283143969341,28.2743338823081),
 .UNSPECIFIED.);
#2082=B_SPLINE_CURVE_WITH_KNOTS('',3,(#27748,#27749,#27750,#27751,#27752,
#27753,#27754,#27755,#27756,#27757,#27758),.UNSPECIFIED.,.F.,.F.,(4,1,1,
1,1,1,1,1,4),(21.9911485751285,22.2404297946851,23.235640669134,24.2308515435829,
25.2260624180317,26.2212732924806,27.2164841669295,28.2116950413783,28.274333882308),
 .UNSPECIFIED.);
#2083=B_SPLINE_CURVE_WITH_KNOTS('',3,(#27763,#27764,#27765,#27766,#27767,
#27768,#27769,#27770,#27771,#27772),.UNSPECIFIED.,.F.,.F.,(4,1,1,1,1,1,
1,4),(15.7079632679489,16.5879333319169,17.5825134287367,18.5770935255564,
19.5716736223762,20.5662537191959,21.5608338160156,21.9911485751285),
 .UNSPECIFIED.);
#2084=B_SPLINE_CURVE_WITH_KNOTS('',3,(#27773,#27774,#27775,#27776,#27777,
#27778,#27779,#27780,#27781,#27782),.UNSPECIFIED.,.F.,.F.,(4,1,1,1,1,1,
1,4),(15.7079632679489,16.2691645479919,17.2643754224408,18.2595862968897,
19.2547971713385,20.2500080457874,21.2452189202363,21.9911485751285),
 .UNSPECIFIED.);
#2085=B_SPLINE_CURVE_WITH_KNOTS('',3,(#27785,#27786,#27787,#27788,#27789,
#27790,#27791,#27792,#27793,#27794,#27795,#27796,#27797,#27798,#27799,#27800,
#27801,#27802,#27803,#27804,#27805,#27806,#27807,#27808,#27809,#27810,#27811,
#27812,#27813,#27814,#27815,#27816,#27817,#27818,#27819,#27820,#27821,#27822,
#27823,#27824,#27825,#27826,#27827,#27828,#27829,#27830,#27831,#27832,#27833,
#27834,#27835,#27836,#27837,#27838,#27839,#27840,#27841,#27842,#27843,#27844,
#27845,#27846,#27847,#27848,#27849,#27850,#27851,#27852,#27853,#27854,#27855,
#27856,#27857,#27858,#27859,#27860,#27861,#27862,#27863,#27864,#27865,#27866,
#27867,#27868,#27869,#27870,#27871,#27872,#27873,#27874,#27875,#27876,#27877,
#27878,#27879,#27880,#27881,#27882,#27883,#27884,#27885,#27886,#27887,#27888,
#27889,#27890,#27891,#27892,#27893,#27894,#27895,#27896,#27897,#27898,#27899,
#27900,#27901,#27902,#27903,#27904,#27905,#27906,#27907,#27908,#27909,#27910,
#27911,#27912,#27913,#27914,#27915,#27916,#27917,#27918,#27919,#27920,#27921,
#27922,#27923,#27924,#27925,#27926,#27927,#27928,#27929,#27930,#27931,#27932,
#27933,#27934,#27935,#27936,#27937,#27938,#27939,#27940,#27941,#27942,#27943,
#27944,#27945,#27946,#27947,#27948,#27949,#27950,#27951,#27952,#27953,#27954,
#27955,#27956,#27957,#27958,#27959,#27960,#27961,#27962,#27963,#27964,#27965,
#27966,#27967,#27968,#27969,#27970,#27971,#27972,#27973,#27974,#27975,#27976,
#27977,#27978,#27979,#27980,#27981,#27982,#27983,#27984,#27985,#27986,#27987,
#27988,#27989,#27990,#27991,#27992,#27993,#27994,#27995,#27996,#27997,#27998,
#27999,#28000,#28001),.UNSPECIFIED.,.F.,.F.,(4,3,3,3,3,3,3,3,3,3,3,3,3,
3,3,3,3,3,3,3,3,3,3,3,3,3,3,3,3,3,3,3,3,3,3,3,3,3,3,3,3,3,3,3,3,3,3,3,3,
3,3,3,3,3,3,3,3,3,3,3,3,3,3,3,3,3,3,3,3,3,3,3,4),(-1.51155304937218,-1.48679589018691,
-1.46138238829548,-1.44932968678137,-1.44202339889261,-1.43723753989169,
-1.41130220328917,-1.38513854317652,-1.36889998110575,-1.36503952627177,
-1.33858827470488,-1.31226992028779,-1.2904045421787,-1.27947185312415,
-1.2739418323947,-1.26910255727935,-1.26853916406961,-1.24320807613995,
-1.21713370060773,-1.19192364256778,-1.1808942421753,-1.17533077231359,
-1.17132639907569,-1.14454252235409,-1.11744879668778,-1.09194990658787,
-1.08205955713065,-1.07541108639849,-1.07098105357362,-1.04321714493087,
-1.01545323628813,-0.988586919757226,-0.977559947169411,-0.973454614695351,
-0.945849052593242,-0.918335863837345,-0.890659863078365,-0.880780750637945,
-0.874611135600851,-0.869075769037592,-0.839959356247813,-0.812088250518227,
-0.784649362472489,-0.774142465660809,-0.769176292614452,-0.765440171794195,
-0.752610117878475,-0.725564556570394,-0.697804528028517,-0.670559901065443,
-0.663513210433686,-0.658766646015375,-0.63051115053422,-0.601912995645473,
-0.573421525171605,-0.561724773565645,-0.556706216040174,-0.552062451237872,
-0.523185606324559,-0.494757836998693,-0.479847512323927,-0.451360048372548,
-0.445014903039589,-0.416674688960391,-0.387739897039467,-0.3585492715235,
-0.342105607427002,-0.337686588976065,-0.308251612910489,-0.278764630960614,
-0.249889482606856,-0.226999958751517,-0.219677966288002),.UNSPECIFIED.);
#2086=B_SPLINE_CURVE_WITH_KNOTS('',3,(#28003,#28004,#28005,#28006,#28007,
#28008,#28009,#28010,#28011,#28012,#28013,#28014,#28015,#28016,#28017,#28018,
#28019,#28020,#28021,#28022,#28023,#28024,#28025,#28026,#28027,#28028,#28029,
#28030,#28031,#28032,#28033,#28034,#28035,#28036,#28037,#28038,#28039,#28040,
#28041,#28042,#28043,#28044,#28045,#28046,#28047,#28048,#28049,#28050,#28051,
#28052,#28053,#28054,#28055,#28056,#28057,#28058,#28059,#28060,#28061,#28062,
#28063,#28064,#28065,#28066),.UNSPECIFIED.,.F.,.F.,(4,3,3,3,3,3,3,3,3,3,
3,3,3,3,3,3,3,3,3,3,3,4),(-0.410648750432968,-0.381297076896285,-0.351072899913787,
-0.328404767176913,-0.311403667624258,-0.306442089482872,-0.302102601213264,
-0.274553556804158,-0.260400368966293,-0.232154047098012,-0.20313479121076,
-0.198616600552917,-0.194415645561828,-0.167218225709786,-0.140141557977483,
-0.113536626964066,-0.0982426601520032,-0.0937832747631835,-0.0680349364798781,
-0.0426775990213316,-0.0180562547442421,0.),.UNSPECIFIED.);
#2087=B_SPLINE_CURVE_WITH_KNOTS('',3,(#28069,#28070,#28071,#28072,#28073,
#28074,#28075,#28076,#28077,#28078,#28079,#28080,#28081,#28082,#28083,#28084,
#28085,#28086,#28087,#28088,#28089,#28090,#28091,#28092,#28093,#28094,#28095,
#28096,#28097,#28098,#28099),.UNSPECIFIED.,.F.,.F.,(4,3,3,3,3,3,3,3,3,3,
4),(-0.219677966288002,-0.197396196086295,-0.168503105981079,-0.139030379252539,
-0.121651581845971,-0.11563839456145,-0.111282058235295,-0.0816044721193899,
-0.0515653636756491,-0.0216265990765453,0.),.UNSPECIFIED.);
#2088=B_SPLINE_CURVE_WITH_KNOTS('',3,(#28612,#28613,#28614,#28615,#28616,
#28617,#28618,#28619),.UNSPECIFIED.,.F.,.F.,(4,1,1,1,1,4),(11.6150328478182,
12.609612944638,13.6041930414577,14.5987731382775,15.5933532350972,15.7079632679489),
 .UNSPECIFIED.);
#2089=B_SPLINE_CURVE_WITH_KNOTS('',3,(#28620,#28621,#28622,#28623,#28624,
#28625,#28626,#28627,#28628,#28629,#28630,#28631,#28632,#28633,#28634,#28635,
#28636,#28637,#28638,#28639,#28640,#28641,#28642,#28643,#28644,#28645,#28646,
#28647,#28648,#28649,#28650,#28651,#28652,#28653,#28654,#28655,#28656,#28657,
#28658,#28659,#28660,#28661,#28662,#28663,#28664,#28665,#28666,#28667,#28668,
#28669,#28670,#28671,#28672,#28673,#28674,#28675,#28676,#28677,#28678,#28679,
#28680,#28681,#28682,#28683,#28684,#28685,#28686,#28687,#28688,#28689,#28690,
#28691,#28692,#28693,#28694,#28695,#28696,#28697,#28698,#28699,#28700,#28701,
#28702,#28703,#28704,#28705,#28706,#28707,#28708,#28709,#28710),
 .UNSPECIFIED.,.F.,.F.,(4,3,3,3,3,3,3,3,3,3,3,3,3,3,3,3,3,3,3,3,3,3,3,3,
3,3,3,3,3,3,4),(-0.552745378375042,-0.529416010123812,-0.500021421858097,
-0.484490821675271,-0.477389212266168,-0.472189171636004,-0.443139563409207,
-0.419188595349667,-0.408465056144172,-0.40220615535047,-0.397553084820015,
-0.369246017540656,-0.339817467888714,-0.312695003632551,-0.296611352770663,
-0.291417321934603,-0.264612611533511,-0.251531818932889,-0.224160792273692,
-0.19614069323948,-0.191761200285163,-0.165152286051105,-0.138522950074249,
-0.112274345430976,-0.0982400522521039,-0.0941400538979384,-0.0901685480379393,
-0.064623178524502,-0.0394785441680361,-0.0151170408359151,0.),
 .UNSPECIFIED.);
#2090=B_SPLINE_CURVE_WITH_KNOTS('',3,(#28711,#28712,#28713,#28714,#28715,
#28716,#28717,#28718,#28719,#28720,#28721,#28722,#28723,#28724,#28725,#28726,
#28727,#28728,#28729),.UNSPECIFIED.,.F.,.F.,(4,3,3,3,3,3,4),(-121.813583759138,
-121.338771812008,-120.344191715188,-119.349611618369,-118.355031521549,
-117.360451424729,-117.190265949363),.UNSPECIFIED.);
#2091=B_SPLINE_CURVE_WITH_KNOTS('',3,(#28732,#28733,#28734,#28735,#28736,
#28737,#28738,#28739,#28740),.UNSPECIFIED.,.F.,.F.,(4,1,1,1,1,1,4),(10.3761157273101,
11.2931101757476,12.2883210501965,13.2835319246454,14.2787427990942,15.2739536735431,
15.7079632679489),.UNSPECIFIED.);
#2092=B_SPLINE_CURVE_WITH_KNOTS('',3,(#29258,#29259,#29260,#29261,#29262,
#29263,#29264,#29265,#29266,#29267,#29268,#29269,#29270,#29271,#29272,#29273,
#29274,#29275,#29276,#29277,#29278,#29279),.UNSPECIFIED.,.F.,.F.,(4,3,3,
3,3,3,3,4),(114.214635937601,114.449250561619,115.444461436068,116.439672310517,
117.434883184966,118.430094059415,119.425304933864,119.744945584229),
 .UNSPECIFIED.);
#2093=B_SPLINE_CURVE_WITH_KNOTS('',3,(#29280,#29281,#29282,#29283,#29284,
#29285,#29286,#29287,#29288,#29289,#29290,#29291,#29292,#29293,#29294,#29295,
#29296,#29297,#29298,#29299,#29300,#29301,#29302,#29303,#29304,#29305,#29306,
#29307,#29308,#29309,#29310,#29311,#29312,#29313,#29314,#29315,#29316,#29317,
#29318,#29319,#29320,#29321,#29322,#29323,#29324,#29325,#29326,#29327,#29328,
#29329,#29330,#29331,#29332,#29333,#29334,#29335,#29336,#29337,#29338,#29339,
#29340,#29341,#29342,#29343,#29344,#29345,#29346,#29347,#29348,#29349,#29350,
#29351,#29352,#29353,#29354,#29355,#29356,#29357,#29358,#29359,#29360,#29361,
#29362,#29363,#29364,#29365,#29366,#29367,#29368,#29369,#29370),
 .UNSPECIFIED.,.F.,.F.,(4,3,3,3,3,3,3,3,3,3,3,3,3,3,3,3,3,3,3,3,3,3,3,3,
3,3,3,3,3,3,4),(-0.555272788399385,-0.536419916279172,-0.511694572405047,
-0.497319076721282,-0.491892658567545,-0.487001163442623,-0.461206429703333,
-0.438766456173517,-0.427478497207602,-0.421962696929991,-0.395379115887254,
-0.366955997281641,-0.345638658327431,-0.329650654111773,-0.325133772019457,
-0.321069591482979,-0.293154594927527,-0.2816866414648,-0.254736587799489,
-0.227248158920029,-0.221184076554202,-0.216726936955391,-0.188773314511124,
-0.160283879462109,-0.131556417226141,-0.114343955822663,-0.109568083488329,
-0.0800957844431539,-0.0505511580101775,-0.0215769774899928,0.),
 .UNSPECIFIED.);
#2094=B_SPLINE_CURVE_WITH_KNOTS('',3,(#29424,#29425,#29426,#29427,#29428,
#29429,#29430,#29431,#29432,#29433),.UNSPECIFIED.,.F.,.F.,(4,3,3,4),(-4.09293042013066,
-3.9493215972006,-2.96199119790045,-2.06863817490914),.UNSPECIFIED.);
#2095=B_SPLINE_CURVE_WITH_KNOTS('',3,(#29436,#29437,#29438,#29439,#29440,
#29441,#29442),.UNSPECIFIED.,.F.,.F.,(4,3,4),(0.,0.988566943725272,1.11730040836823),
 .UNSPECIFIED.);
#2096=B_SPLINE_CURVE_WITH_KNOTS('',3,(#29447,#29448,#29449,#29450,#29451,
#29452,#29453,#29454,#29455,#29456,#29457,#29458,#29459,#29460,#29461,#29462,
#29463,#29464,#29465,#29466,#29467,#29468),.UNSPECIFIED.,.F.,.F.,(4,3,3,
3,3,3,3,4),(-10.3761157273102,-9.87330399300149,-8.88597359370134,-7.89864319440119,
-6.91131279510104,-5.92398239580089,-4.93665199650074,-4.09293042013066),
 .UNSPECIFIED.);
#2097=B_SPLINE_CURVE_WITH_KNOTS('',3,(#29469,#29470,#29471,#29472,#29473,
#29474,#29475,#29476,#29477,#29478,#29479,#29480,#29481,#29482,#29483,#29484,
#29485,#29486,#29487,#29488,#29489,#29490),.UNSPECIFIED.,.F.,.F.,(4,3,3,
3,3,3,3,4),(1.11730040836823,1.97713388745054,2.9657008311758,3.95426777490106,
4.94283471862632,5.93140166235159,6.91996860607685,7.40048571554782),
 .UNSPECIFIED.);
#2098=B_SPLINE_CURVE_WITH_KNOTS('',3,(#29495,#29496,#29497,#29498,#29499,
#29500,#29501,#29502,#29503,#29504,#29505,#29506,#29507,#29508,#29509,#29510,
#29511,#29512,#29513,#29514,#29515,#29516),.UNSPECIFIED.,.F.,.F.,(4,3,3,
3,3,3,3,4),(-16.6593010344898,-15.7972863888024,-14.8099559895022,-13.8226255902021,
-12.8352951909019,-11.8479647916018,-10.8606343923016,-10.3761157273102),
 .UNSPECIFIED.);
#2099=B_SPLINE_CURVE_WITH_KNOTS('',3,(#29517,#29518,#29519,#29520,#29521,
#29522,#29523,#29524,#29525,#29526,#29527,#29528,#29529,#29530,#29531,#29532,
#29533,#29534,#29535,#29536,#29537,#29538),.UNSPECIFIED.,.F.,.F.,(4,3,3,
3,3,3,3,4),(7.40048571554782,7.90853554980211,8.89710249352738,9.88566943725264,
10.8742363809779,11.8628033247032,12.8513702684284,13.6836710227274),
 .UNSPECIFIED.);
#2100=B_SPLINE_CURVE_WITH_KNOTS('',3,(#29543,#29544,#29545,#29546,#29547,
#29548,#29549,#29550,#29551,#29552,#29553,#29554,#29555,#29556,#29557,#29558,
#29559,#29560,#29561,#29562,#29563,#29564,#29565,#29566,#29567),
 .UNSPECIFIED.,.F.,.F.,(4,3,3,3,3,3,3,3,4),(-22.9424863416694,-22.7085991839034,
-21.7212687846033,-20.7339383853031,-19.746607986003,-18.7592775867028,
-17.7719471874027,-16.7846167881025,-16.6593010344898),.UNSPECIFIED.);
#2101=B_SPLINE_CURVE_WITH_KNOTS('',3,(#29568,#29569,#29570,#29571,#29572,
#29573,#29574,#29575,#29576,#29577,#29578,#29579,#29580,#29581,#29582,#29583,
#29584,#29585,#29586,#29587,#29588,#29589,#29590,#29591,#29592),
 .UNSPECIFIED.,.F.,.F.,(4,3,3,3,3,3,3,3,4),(13.6836710227274,13.8399372121537,
14.828504155879,15.8170710996042,16.8056380433295,17.7942049870548,18.78277193078,
19.7713388745053,19.966856329907),.UNSPECIFIED.);
#2102=B_SPLINE_CURVE_WITH_KNOTS('',3,(#29597,#29598,#29599,#29600,#29601,
#29602,#29603,#29604,#29605,#29606,#29607,#29608,#29609,#29610,#29611,#29612,
#29613,#29614,#29615,#29616,#29617,#29618),.UNSPECIFIED.,.F.,.F.,(4,3,3,
3,3,3,3,4),(-29.225671648849,-28.6325815797043,-27.6452511804042,-26.657920781104,
-25.6705903818039,-24.6832599825037,-23.6959295832036,-22.9424863416694),
 .UNSPECIFIED.);
#2103=B_SPLINE_CURVE_WITH_KNOTS('',3,(#29619,#29620,#29621,#29622,#29623,
#29624,#29625,#29626,#29627,#29628,#29629,#29630,#29631,#29632,#29633,#29634,
#29635,#29636,#29637,#29638,#29639,#29640),.UNSPECIFIED.,.F.,.F.,(4,3,3,
3,3,3,3,4),(19.966856329907,20.7599058182306,21.7484727619558,22.7370397056811,
23.7256066494064,24.7141735931316,25.7027405368569,26.2500416370866),
 .UNSPECIFIED.);
#2104=B_SPLINE_CURVE_WITH_KNOTS('',3,(#29645,#29646,#29647,#29648,#29649,
#29650,#29651,#29652,#29653,#29654,#29655,#29656,#29657,#29658,#29659,#29660,
#29661,#29662,#29663,#29664,#29665,#29666),.UNSPECIFIED.,.F.,.F.,(4,3,3,
3,3,3,3,4),(-35.5088569560286,-34.5565639755052,-33.5692335762051,-32.5819031769049,
-31.5945727776048,-30.6072423783046,-29.6199119790045,-29.225671648849),
 .UNSPECIFIED.);
#2105=B_SPLINE_CURVE_WITH_KNOTS('',3,(#29667,#29668,#29669,#29670,#29671,
#29672,#29673,#29674,#29675,#29676,#29677,#29678,#29679,#29680,#29681,#29682,
#29683,#29684,#29685,#29686,#29687,#29688),.UNSPECIFIED.,.F.,.F.,(4,3,3,
3,3,3,3,4),(26.2500416370866,26.6913074805822,27.6798744243074,28.6684413680327,
29.6570083117579,30.6455752554832,31.6341421992085,32.5332269442662),
 .UNSPECIFIED.);
#2106=B_SPLINE_CURVE_WITH_KNOTS('',3,(#29693,#29694,#29695,#29696,#29697,
#29698,#29699,#29700,#29701,#29702,#29703,#29704,#29705,#29706,#29707,#29708,
#29709,#29710,#29711,#29712,#29713,#29714,#29715,#29716,#29717),
 .UNSPECIFIED.,.F.,.F.,(4,3,3,3,3,3,3,3,4),(-41.7920422632082,-41.4678767706063,
-40.4805463713061,-39.4932159720059,-38.5058855727058,-37.5185551734057,
-36.5312247741055,-35.5438943748054,-35.5088569560286),.UNSPECIFIED.);
#2107=B_SPLINE_CURVE_WITH_KNOTS('',3,(#29718,#29719,#29720,#29721,#29722,
#29723,#29724,#29725,#29726,#29727,#29728,#29729,#29730,#29731,#29732,#29733,
#29734,#29735,#29736,#29737,#29738,#29739,#29740,#29741,#29742),
 .UNSPECIFIED.,.F.,.F.,(4,3,3,3,3,3,3,3,4),(32.5332269442662,32.6227091429337,
33.611276086659,34.5998430303843,35.5884099741095,36.5769769178348,37.5655438615601,
38.5541108052853,38.8164122514458),.UNSPECIFIED.);
#2108=B_SPLINE_CURVE_WITH_KNOTS('',3,(#29747,#29748,#29749,#29750,#29751,
#29752,#29753,#29754,#29755,#29756,#29757,#29758,#29759,#29760,#29761,#29762,
#29763,#29764,#29765,#29766,#29767,#29768),.UNSPECIFIED.,.F.,.F.,(4,3,3,
3,3,3,3,4),(-48.0752275703878,-47.3918591664071,-46.404528767107,-45.4171983678069,
-44.4298679685067,-43.4425375692066,-42.4552071699064,-41.7920422632082),
 .UNSPECIFIED.);
#2109=B_SPLINE_CURVE_WITH_KNOTS('',3,(#29769,#29770,#29771,#29772,#29773,
#29774,#29775,#29776,#29777,#29778,#29779,#29780,#29781,#29782,#29783,#29784,
#29785,#29786,#29787,#29788,#29789,#29790),.UNSPECIFIED.,.F.,.F.,(4,3,3,
3,3,3,3,4),(38.8164122514458,39.5426777490106,40.5312446927359,41.5198116364611,
42.5083785801864,43.4969455239117,44.4855124676369,45.0995975586253),
 .UNSPECIFIED.);
#2110=B_SPLINE_CURVE_WITH_KNOTS('',3,(#29795,#29796,#29797,#29798,#29799,
#29800,#29801,#29802,#29803,#29804,#29805,#29806,#29807,#29808,#29809,#29810,
#29811,#29812,#29813,#29814,#29815,#29816,#29817,#29818,#29819),
 .UNSPECIFIED.,.F.,.F.,(4,3,3,3,3,3,3,3,4),(-54.3584128775674,-54.3031719615082,
-53.315841562208,-52.3285111629079,-51.3411807636077,-50.3538503643076,
-49.3665199650074,-48.3791895657073,-48.0752275703878),.UNSPECIFIED.);
#2111=B_SPLINE_CURVE_WITH_KNOTS('',3,(#29820,#29821,#29822,#29823,#29824,
#29825,#29826,#29827,#29828,#29829,#29830,#29831,#29832,#29833,#29834,#29835,
#29836,#29837,#29838,#29839,#29840,#29841),.UNSPECIFIED.,.F.,.F.,(4,3,3,
3,3,3,3,4),(45.0995975586253,45.4740794113622,46.4626463550875,47.4512132988127,
48.439780242538,49.4283471862633,50.4169141299885,51.3827828658049),
 .UNSPECIFIED.);
#2112=B_SPLINE_CURVE_WITH_KNOTS('',3,(#29846,#29847,#29848,#29849,#29850,
#29851,#29852,#29853,#29854,#29855,#29856,#29857,#29858,#29859,#29860,#29861,
#29862,#29863,#29864,#29865,#29866,#29867),.UNSPECIFIED.,.F.,.F.,(4,3,3,
3,3,3,3,4),(-60.641598184747,-60.2271543573091,-59.2398239580089,-58.2524935587088,
-57.2651631594086,-56.2778327601085,-55.2905023608083,-54.3584128775674),
 .UNSPECIFIED.);
#2113=B_SPLINE_CURVE_WITH_KNOTS('',3,(#29868,#29869,#29870,#29871,#29872,
#29873,#29874,#29875,#29876,#29877,#29878,#29879,#29880,#29881,#29882,#29883,
#29884,#29885,#29886,#29887,#29888,#29889,#29890,#29891,#29892),
 .UNSPECIFIED.,.F.,.F.,(4,3,3,3,3,3,3,3,4),(51.3827828658049,51.4054810737138,
52.394048017439,53.3826149611643,54.3711819048896,55.3597488486148,56.3483157923401,
57.3368827360654,57.6659681729845),.UNSPECIFIED.);
#2114=B_SPLINE_CURVE_WITH_KNOTS('',3,(#29897,#29898,#29899,#29900,#29901,
#29902,#29903,#29904,#29905,#29906,#29907,#29908,#29909,#29910,#29911,#29912,
#29913,#29914,#29915,#29916,#29917,#29918),.UNSPECIFIED.,.F.,.F.,(4,3,3,
3,3,3,3,4),(-66.9247834919266,-66.15113675311,-65.1638063538098,-64.1764759545097,
-63.1891455552095,-62.2018151559094,-61.2144847566092,-60.641598184747),
 .UNSPECIFIED.);
#2115=B_SPLINE_CURVE_WITH_KNOTS('',3,(#29919,#29920,#29921,#29922,#29923,
#29924,#29925,#29926,#29927,#29928,#29929,#29930,#29931,#29932,#29933,#29934,
#29935,#29936,#29937,#29938,#29939,#29940),.UNSPECIFIED.,.F.,.F.,(4,3,3,
3,3,3,3,4),(57.6659681729845,58.3254496797906,59.3140166235159,60.3025835672412,
61.2911505109664,62.2797174546917,63.268284398417,63.9491534801641),
 .UNSPECIFIED.);
#2116=B_SPLINE_CURVE_WITH_KNOTS('',3,(#29946,#29947,#29948,#29949,#29950,
#29951,#29952,#29953,#29954,#29955),.UNSPECIFIED.,.F.,.F.,(4,1,1,1,1,1,
1,4),(78.5398163397448,78.7535000002284,79.7408303995285,80.7281607988287,
81.7154911981288,82.702821597429,83.6901519967291,84.6774823960293),
 .UNSPECIFIED.);
#2117=B_SPLINE_CURVE_WITH_KNOTS('',3,(#29958,#29959,#29960,#29961,#29962,
#29963,#29964,#29965),.UNSPECIFIED.,.F.,.F.,(4,1,1,1,1,4),(78.5398163397448,
79.4842975006201,80.4728644443454,81.4614313880706,82.4499983317959,83.4385652755212),
 .UNSPECIFIED.);
#2118=B_SPLINE_CURVE_WITH_KNOTS('',3,(#29970,#29971,#29972,#29973,#29974,
#29975,#29976,#29977,#29978,#29979),.UNSPECIFIED.,.F.,.F.,(4,1,1,1,1,1,
1,4),(72.2566310325653,72.8295176044275,73.8168480037276,74.8041784030278,
75.7915088023279,76.7788392016281,77.7661696009282,78.5398163397448),
 .UNSPECIFIED.);
#2119=B_SPLINE_CURVE_WITH_KNOTS('',3,(#29980,#29981,#29982,#29983,#29984,
#29985,#29986,#29987,#29988,#29989,#29990),.UNSPECIFIED.,.F.,.F.,(4,1,1,
1,1,1,1,1,4),(72.2566310325652,72.5643288945433,73.5528958382685,74.5414627819938,
75.530029725719,76.5185966694443,77.5071636131696,78.4957305568948,78.5398163397448),
 .UNSPECIFIED.);
#2120=B_SPLINE_CURVE_WITH_KNOTS('',3,(#29995,#29996,#29997,#29998,#29999,
#30000,#30001,#30002,#30003,#30004),.UNSPECIFIED.,.F.,.F.,(4,1,1,1,1,1,
1,4),(65.9734457253856,66.9055352086266,67.8928656079267,68.8801960072269,
69.867526406527,70.8548568058272,71.8421872051273,72.2566310325653),
 .UNSPECIFIED.);
#2121=B_SPLINE_CURVE_WITH_KNOTS('',3,(#30005,#30006,#30007,#30008,#30009,
#30010,#30011,#30012,#30013,#30014),.UNSPECIFIED.,.F.,.F.,(4,1,1,1,1,1,
1,4),(65.9734457253856,66.6329272321917,67.6214941759169,68.6100611196422,
69.5986280633675,70.5871950070927,71.575761950818,72.2566310325652),
 .UNSPECIFIED.);
#2122=B_SPLINE_CURVE_WITH_KNOTS('',3,(#30019,#30020,#30021,#30022,#30023,
#30024,#30025,#30026,#30027,#30028,#30029),.UNSPECIFIED.,.F.,.F.,(4,1,1,
1,1,1,1,1,4),(59.6902604182061,59.9942224135255,60.9815528128257,61.9688832121258,
62.956213611426,63.9435440107261,64.9308744100263,65.9182048093264,65.9734457253856),
 .UNSPECIFIED.);
#2123=B_SPLINE_CURVE_WITH_KNOTS('',3,(#30030,#30031,#30032,#30033,#30034,
#30035,#30036,#30037,#30038,#30039,#30040),.UNSPECIFIED.,.F.,.F.,(4,1,1,
1,1,1,1,1,4),(59.6902604182061,59.7129586261148,60.7015255698401,61.6900925135653,
62.6786594572906,63.6672264010159,64.6557933447411,65.6443602884664,65.9734457253856),
 .UNSPECIFIED.);
#2124=B_SPLINE_CURVE_WITH_KNOTS('',3,(#30045,#30046,#30047,#30048,#30049,
#30050,#30051,#30052,#30053,#30054),.UNSPECIFIED.,.F.,.F.,(4,1,1,1,1,1,
1,4),(53.4070751110265,54.0702400177247,55.0575704170248,56.0449008163249,
57.0322312156251,58.0195616149252,59.0068920142254,59.6902604182061),
 .UNSPECIFIED.);
#2125=B_SPLINE_CURVE_WITH_KNOTS('',3,(#30055,#30056,#30057,#30058,#30059,
#30060,#30061,#30062,#30063,#30064),.UNSPECIFIED.,.F.,.F.,(4,1,1,1,1,1,
1,4),(53.4070751110265,53.7815569637632,54.7701239074885,55.7586908512138,
56.747257794939,57.7358247386643,58.7243916823895,59.6902604182061),
 .UNSPECIFIED.);
#2126=B_SPLINE_CURVE_WITH_KNOTS('',3,(#30069,#30070,#30071,#30072,#30073,
#30074,#30075,#30076,#30077,#30078,#30079),.UNSPECIFIED.,.F.,.F.,(4,1,1,
1,1,1,1,1,4),(47.1238898038469,47.1589272226236,48.1462576219238,49.1335880212239,
50.1209184205241,51.1082488198242,52.0955792191244,53.0829096184245,53.4070751110265),
 .UNSPECIFIED.);
#2127=B_SPLINE_CURVE_WITH_KNOTS('',3,(#30080,#30081,#30082,#30083,#30084,
#30085,#30086,#30087,#30088,#30089),.UNSPECIFIED.,.F.,.F.,(4,1,1,1,1,1,
1,4),(47.1238898038469,47.8501553014116,48.8387222451369,49.8272891888622,
50.8158561325874,51.8044230763127,52.792990020038,53.4070751110265),
 .UNSPECIFIED.);
#2128=B_SPLINE_CURVE_WITH_KNOTS('',3,(#30094,#30095,#30096,#30097,#30098,
#30099,#30100,#30101,#30102,#30103),.UNSPECIFIED.,.F.,.F.,(4,1,1,1,1,1,
1,4),(40.8407044966673,41.2349448268227,42.2222752261229,43.209605625423,
44.1969360247232,45.1842664240233,46.1715968233235,47.1238898038469),
 .UNSPECIFIED.);
#2129=B_SPLINE_CURVE_WITH_KNOTS('',3,(#30104,#30105,#30106,#30107,#30108,
#30109,#30110,#30111,#30112,#30113,#30114),.UNSPECIFIED.,.F.,.F.,(4,1,1,
1,1,1,1,1,4),(40.8407044966673,40.9301866953348,41.91875363906,42.9073205827853,
43.8958875265106,44.8844544702358,45.8730214139611,46.8615883576864,47.1238898038469),
 .UNSPECIFIED.);
#2130=B_SPLINE_CURVE_WITH_KNOTS('',3,(#30119,#30120,#30121,#30122,#30123,
#30124,#30125,#30126,#30127,#30128),.UNSPECIFIED.,.F.,.F.,(4,1,1,1,1,1,
1,4),(34.5575191894877,35.3109624310218,36.298292830322,37.2856232296221,
38.2729536289223,39.2602840282224,40.2476144275226,40.8407044966673),
 .UNSPECIFIED.);
#2131=B_SPLINE_CURVE_WITH_KNOTS('',3,(#30129,#30130,#30131,#30132,#30133,
#30134,#30135,#30136,#30137,#30138),.UNSPECIFIED.,.F.,.F.,(4,1,1,1,1,1,
1,4),(34.5575191894877,34.9987850329832,35.9873519767085,36.9759189204337,
37.964485864159,38.9530528078842,39.9416197516095,40.8407044966673),
 .UNSPECIFIED.);
#2132=B_SPLINE_CURVE_WITH_KNOTS('',3,(#30143,#30144,#30145,#30146,#30147,
#30148,#30149,#30150,#30151,#30152,#30153),.UNSPECIFIED.,.F.,.F.,(4,1,1,
1,1,1,1,1,4),(28.2743338823081,28.3996496359208,29.3869800352209,30.3743104345211,
31.3616408338212,32.3489712331214,33.3363016324215,34.3236320317217,34.5575191894877),
 .UNSPECIFIED.);
#2133=B_SPLINE_CURVE_WITH_KNOTS('',3,(#30154,#30155,#30156,#30157,#30158,
#30159,#30160,#30161,#30162,#30163),.UNSPECIFIED.,.F.,.F.,(4,1,1,1,1,1,
1,4),(28.2743338823081,29.0673833706316,30.0559503143569,31.0445172580821,
32.0330842018074,33.0216511455327,34.0102180892579,34.5575191894877),
 .UNSPECIFIED.);
#2134=B_SPLINE_CURVE_WITH_KNOTS('',3,(#30168,#30169,#30170,#30171,#30172,
#30173,#30174,#30175,#30176,#30177),.UNSPECIFIED.,.F.,.F.,(4,1,1,1,1,1,
1,4),(21.9911485751285,22.4756672401199,23.46299763942,24.4503280387202,
25.4376584380203,26.4249888373205,27.4123192366206,28.2743338823081),
 .UNSPECIFIED.);
#2135=B_SPLINE_CURVE_WITH_KNOTS('',3,(#30178,#30179,#30180,#30181,#30182,
#30183,#30184,#30185,#30186,#30187,#30188),.UNSPECIFIED.,.F.,.F.,(4,1,1,
1,1,1,1,1,4),(21.9911485751285,22.1474147645547,23.13598170828,24.1245486520053,
25.1131155957305,26.1016825394558,27.0902494831811,28.0788164269063,28.2743338823081),
 .UNSPECIFIED.);
#2136=B_SPLINE_CURVE_WITH_KNOTS('',3,(#30193,#30194,#30195,#30196,#30197,
#30198,#30199,#30200,#30201,#30202),.UNSPECIFIED.,.F.,.F.,(4,1,1,1,1,1,
1,4),(15.7079632679489,16.551684844319,17.5390152436191,18.5263456429193,
19.5136760422194,20.5010064415196,21.4883368408197,21.9911485751285),
 .UNSPECIFIED.);
#2137=B_SPLINE_CURVE_WITH_KNOTS('',3,(#30203,#30204,#30205,#30206,#30207,
#30208,#30209,#30210,#30211,#30212),.UNSPECIFIED.,.F.,.F.,(4,1,1,1,1,1,
1,4),(15.7079632679489,16.2160131022032,17.2045800459284,18.1931469896537,
19.181713933379,20.1702808771042,21.1588478208295,21.9911485751285),
 .UNSPECIFIED.);
#2138=B_SPLINE_CURVE_WITH_KNOTS('',3,(#30215,#30216,#30217,#30218,#30219,
#30220,#30221,#30222,#30223,#30224,#30225,#30226,#30227,#30228,#30229,#30230,
#30231,#30232,#30233,#30234,#30235,#30236,#30237,#30238,#30239,#30240,#30241,
#30242,#30243,#30244,#30245,#30246,#30247,#30248,#30249,#30250,#30251,#30252,
#30253,#30254,#30255,#30256,#30257,#30258,#30259,#30260,#30261,#30262,#30263,
#30264,#30265,#30266,#30267,#30268,#30269,#30270,#30271,#30272,#30273,#30274,
#30275,#30276,#30277,#30278,#30279,#30280,#30281,#30282,#30283,#30284,#30285,
#30286,#30287,#30288,#30289,#30290,#30291,#30292,#30293,#30294,#30295,#30296,
#30297,#30298,#30299,#30300,#30301,#30302,#30303,#30304,#30305,#30306,#30307,
#30308,#30309,#30310,#30311,#30312,#30313,#30314,#30315,#30316,#30317,#30318,
#30319,#30320,#30321,#30322,#30323,#30324,#30325,#30326,#30327,#30328,#30329,
#30330,#30331,#30332,#30333,#30334,#30335,#30336,#30337,#30338,#30339,#30340,
#30341,#30342,#30343,#30344,#30345,#30346,#30347,#30348,#30349,#30350,#30351,
#30352,#30353,#30354,#30355,#30356,#30357,#30358,#30359,#30360,#30361,#30362,
#30363,#30364,#30365,#30366,#30367,#30368,#30369,#30370,#30371,#30372,#30373,
#30374,#30375,#30376,#30377,#30378,#30379,#30380,#30381,#30382,#30383,#30384,
#30385,#30386,#30387,#30388,#30389,#30390,#30391,#30392,#30393,#30394,#30395,
#30396,#30397,#30398,#30399,#30400,#30401,#30402,#30403,#30404,#30405,#30406,
#30407,#30408,#30409,#30410,#30411,#30412,#30413,#30414,#30415,#30416,#30417,
#30418,#30419,#30420,#30421,#30422,#30423,#30424,#30425,#30426,#30427,#30428,
#30429,#30430,#30431),.UNSPECIFIED.,.F.,.F.,(4,3,3,3,3,3,3,3,3,3,3,3,3,
3,3,3,3,3,3,3,3,3,3,3,3,3,3,3,3,3,3,3,3,3,3,3,3,3,3,3,3,3,3,3,3,3,3,3,3,
3,3,3,3,3,3,3,3,3,3,3,3,3,3,3,3,3,3,3,3,3,3,3,4),(-1.51155304937228,-1.48679174718013,
-1.46137597198077,-1.44942691521821,-1.44205848651244,-1.43724119559823,
-1.41130764113729,-1.38514768961224,-1.36936593028954,-1.36512230166791,
-1.33867581137855,-1.31235917608035,-1.29127511993008,-1.28073309185494,
-1.2739086628828,-1.27019106377981,-1.24488979836553,-1.21884130205047,
-1.19384888620637,-1.18291470427457,-1.17641188206357,-1.17130697868968,
-1.14451640582175,-1.11742561305122,-1.09279470361283,-1.08177565945417,
-1.07670730294613,-1.07245364414871,-1.0452101587782,-1.01890197529764,
-0.992076665792053,-0.977095538498891,-0.971310437727824,-0.944262984582137,
-0.91671696123902,-0.889051349044572,-0.8786107219546,-0.873404326505122,
-0.869185758667877,-0.841205731090746,-0.813331817877821,-0.785648584359967,
-0.771436006282574,-0.765308450445371,-0.757965350842113,-0.731019445974318,
-0.703340715547858,-0.676331238706378,-0.668063308133434,-0.663247880961674,
-0.658967945513649,-0.630690110839631,-0.602089962339152,-0.573383696958367,
-0.562618847440572,-0.556352694911719,-0.55203012393032,-0.523164492059728,
-0.494713544949419,-0.487264900816012,-0.45884309987075,-0.449622389577847,
-0.445165938771905,-0.416742684601646,-0.387755299334011,-0.358563756837841,
-0.34211828207705,-0.337697582134308,-0.308241853281341,-0.278784672736061,
-0.25000255453776,-0.226999958751515,-0.219677966288006),.UNSPECIFIED.);
#2139=B_SPLINE_CURVE_WITH_KNOTS('',3,(#30433,#30434,#30435,#30436,#30437,
#30438,#30439,#30440,#30441,#30442,#30443,#30444,#30445,#30446,#30447,#30448,
#30449,#30450,#30451,#30452,#30453,#30454,#30455,#30456,#30457,#30458,#30459,
#30460,#30461,#30462,#30463,#30464,#30465,#30466,#30467,#30468,#30469,#30470,
#30471,#30472,#30473,#30474,#30475,#30476,#30477,#30478,#30479,#30480,#30481,
#30482,#30483,#30484,#30485,#30486,#30487,#30488,#30489,#30490,#30491,#30492,
#30493),.UNSPECIFIED.,.F.,.F.,(4,3,3,3,3,3,3,3,3,3,3,3,3,3,3,3,3,3,3,3,
4),(-0.410648750432938,-0.381294613665594,-0.352267124576947,-0.328792823836752,
-0.311187098281605,-0.306018425011984,-0.301691296836585,-0.274143229574461,
-0.258369921616165,-0.230117472373342,-0.201352788326674,-0.195525900786732,
-0.16833922287309,-0.141249160586392,-0.114615533759621,-0.100282139063474,
-0.0960342097686789,-0.0702554174629941,-0.0448546715641945,-0.0201984500449382,
0.),.UNSPECIFIED.);
#2140=B_SPLINE_CURVE_WITH_KNOTS('',3,(#30496,#30497,#30498,#30499,#30500,
#30501,#30502,#30503,#30504,#30505,#30506,#30507,#30508,#30509,#30510,#30511,
#30512,#30513,#30514,#30515,#30516,#30517,#30518,#30519,#30520,#30521,#30522,
#30523,#30524,#30525,#30526),.UNSPECIFIED.,.F.,.F.,(4,3,3,3,3,3,3,3,3,3,
4),(-0.219677966288006,-0.206985183547511,-0.178213580556878,-0.148819200354015,
-0.130216800309763,-0.118450459252591,-0.113866160083042,-0.0841488051349767,
-0.0540951018364117,-0.0242019686830237,0.),.UNSPECIFIED.);
#2141=B_SPLINE_CURVE_WITH_KNOTS('',3,(#30839,#30840,#30841,#30842,#30843,
#30844,#30845,#30846),.UNSPECIFIED.,.F.,.F.,(4,1,1,1,1,4),(11.6150328478182,
12.6023632471184,13.5896936464185,14.5770240457187,15.5643544450188,15.7079632679489),
 .UNSPECIFIED.);
#2142=B_SPLINE_CURVE_WITH_KNOTS('',3,(#30847,#30848,#30849,#30850,#30851,
#30852,#30853,#30854,#30855,#30856,#30857,#30858,#30859,#30860,#30861,#30862,
#30863,#30864,#30865,#30866,#30867,#30868,#30869,#30870,#30871,#30872,#30873,
#30874,#30875,#30876,#30877,#30878,#30879,#30880,#30881,#30882,#30883,#30884,
#30885,#30886,#30887,#30888,#30889,#30890,#30891,#30892,#30893,#30894,#30895,
#30896,#30897,#30898,#30899,#30900,#30901,#30902,#30903,#30904,#30905,#30906,
#30907,#30908,#30909,#30910,#30911,#30912,#30913,#30914,#30915,#30916,#30917,
#30918,#30919,#30920,#30921,#30922,#30923,#30924,#30925,#30926,#30927,#30928,
#30929,#30930,#30931,#30932,#30933,#30934),.UNSPECIFIED.,.F.,.F.,(4,3,3,
3,3,3,3,3,3,3,3,3,3,3,3,3,3,3,3,3,3,3,3,3,3,3,3,3,3,4),(-0.55274537837504,
-0.525174630400016,-0.495740003900857,-0.479498227927527,-0.472105972866577,
-0.443064611280178,-0.418881458903182,-0.408301329738247,-0.401969450637142,
-0.397429868442983,-0.369124488132221,-0.341064938672273,-0.313899750226951,
-0.29772704364586,-0.291366968188088,-0.264559598151202,-0.249599392264211,
-0.222215347947115,-0.194438429453726,-0.189292991414398,-0.162670593649827,
-0.136062352557756,-0.109859916217256,-0.101879142728474,-0.0950850259724172,
-0.09115324392662,-0.0655931049079899,-0.0404250325776628,-0.0160423336449029,
0.),.UNSPECIFIED.);
#2143=B_SPLINE_CURVE_WITH_KNOTS('',3,(#30935,#30936,#30937,#30938,#30939,
#30940,#30941,#30942,#30943,#30944,#30945,#30946,#30947,#30948,#30949,#30950,
#30951,#30952,#30953),.UNSPECIFIED.,.F.,.F.,(4,3,3,3,3,3,4),(-71.548101301701,
-71.0877887496107,-70.1004583503106,-69.1131279510104,-68.1257975517103,
-67.1384671524101,-66.9247834919266),.UNSPECIFIED.);
#2144=B_SPLINE_CURVE_WITH_KNOTS('',3,(#30956,#30957,#30958,#30959,#30960,
#30961,#30962,#30963,#30964),.UNSPECIFIED.,.F.,.F.,(4,1,1,1,1,1,4),(10.3761157273102,
11.2731783835768,12.2617453273021,13.2503122710274,14.2388792147526,15.2274461584779,
15.7079632679489),.UNSPECIFIED.);
#2145=B_SPLINE_CURVE_WITH_KNOTS('',3,(#31282,#31283,#31284,#31285,#31286,
#31287,#31288,#31289,#31290,#31291,#31292,#31293,#31294,#31295,#31296,#31297,
#31298,#31299,#31300,#31301,#31302,#31303),.UNSPECIFIED.,.F.,.F.,(4,3,3,
3,3,3,3,4),(63.9491534801641,64.2568513421422,65.2454182858675,66.2339852295928,
67.222552173318,68.2111191170433,69.1996860607685,69.4794631267919),
 .UNSPECIFIED.);
#2146=B_SPLINE_CURVE_WITH_KNOTS('',3,(#31304,#31305,#31306,#31307,#31308,
#31309,#31310,#31311,#31312,#31313,#31314,#31315,#31316,#31317,#31318,#31319,
#31320,#31321,#31322,#31323,#31324,#31325,#31326,#31327,#31328,#31329,#31330,
#31331,#31332,#31333,#31334,#31335,#31336,#31337,#31338,#31339,#31340,#31341,
#31342,#31343,#31344,#31345,#31346,#31347,#31348,#31349,#31350,#31351,#31352,
#31353,#31354,#31355,#31356,#31357,#31358,#31359,#31360,#31361,#31362,#31363,
#31364,#31365,#31366,#31367,#31368,#31369,#31370,#31371,#31372,#31373,#31374,
#31375,#31376,#31377,#31378,#31379,#31380,#31381,#31382,#31383,#31384,#31385,
#31386,#31387,#31388,#31389,#31390,#31391),.UNSPECIFIED.,.F.,.F.,(4,3,3,
3,3,3,3,3,3,3,3,3,3,3,3,3,3,3,3,3,3,3,3,3,3,3,3,3,3,4),(-0.555272788399385,
-0.533197712400843,-0.50841200558917,-0.492097097422296,-0.487698425831477,
-0.461722637175749,-0.438993822101987,-0.427671428401512,-0.42202191869945,
-0.395458071621424,-0.368431943977533,-0.346296987129563,-0.329695769493585,
-0.32517826205158,-0.321068892319616,-0.293156561268766,-0.279892116585652,
-0.25291117159626,-0.225403496298925,-0.221057334466692,-0.216708298034074,
-0.188764735094145,-0.160284152968102,-0.131561788206246,-0.114355289595352,
-0.109564750157472,-0.0800994390258527,-0.050557237845911,-0.0215776241374192,
0.),.UNSPECIFIED.);
#2147=B_SPLINE_CURVE_WITH_KNOTS('',3,(#31460,#31461,#31462,#31463),
 .UNSPECIFIED.,.F.,.F.,(4,4),(32.725489676875,33.4328714289264),
 .UNSPECIFIED.);
#2148=B_SPLINE_CURVE_WITH_KNOTS('',3,(#31466,#31467,#31468,#31469,#31470,
#31471,#31472,#31473,#31474,#31475),.UNSPECIFIED.,.F.,.F.,(4,3,3,4),(-31.4159265358979,
-30.4829121851976,-29.499592437288,-28.9817156343595),.UNSPECIFIED.);
#2149=B_SPLINE_CURVE_WITH_KNOTS('',3,(#31480,#31481,#31482,#31483,#31484,
#31485,#31486,#31487,#31488,#31489,#31490,#31491,#31492,#31493,#31494,#31495,
#31496,#31497,#31498,#31499,#31500,#31501,#31502,#31503,#31504),
 .UNSPECIFIED.,.F.,.F.,(4,3,3,3,3,3,3,3,4),(26.4423043696954,26.5496331935592,
27.5329529414688,28.5162726893784,29.499592437288,30.4829121851976,31.4662319331072,
32.4495516810168,32.725489676875),.UNSPECIFIED.);
#2150=B_SPLINE_CURVE_WITH_KNOTS('',3,(#31505,#31506,#31507,#31508,#31509,
#31510,#31511,#31512,#31513,#31514,#31515,#31516,#31517,#31518,#31519,#31520,
#31521,#31522,#31523,#31524,#31525,#31526),.UNSPECIFIED.,.F.,.F.,(4,3,3,
3,3,3,3,4),(-28.9817156343595,-28.5162726893784,-27.5329529414688,-26.5496331935592,
-25.5663134456496,-24.58299369774,-23.5996739498304,-22.6985303271799),
 .UNSPECIFIED.);
#2151=B_SPLINE_CURVE_WITH_KNOTS('',3,(#31531,#31532,#31533,#31534,#31535,
#31536,#31537,#31538,#31539,#31540,#31541,#31542,#31543,#31544,#31545,#31546,
#31547,#31548,#31549,#31550,#31551,#31552),.UNSPECIFIED.,.F.,.F.,(4,3,3,
3,3,3,3,4),(20.1591190625159,20.6497147061016,21.6330344540112,22.6163542019208,
23.5996739498304,24.58299369774,25.5663134456496,26.4423043696954),
 .UNSPECIFIED.);
#2152=B_SPLINE_CURVE_WITH_KNOTS('',3,(#31553,#31554,#31555,#31556,#31557,
#31558,#31559,#31560,#31561,#31562,#31563,#31564,#31565,#31566,#31567,#31568,
#31569,#31570,#31571,#31572,#31573,#31574,#31575,#31576,#31577),
 .UNSPECIFIED.,.F.,.F.,(4,3,3,3,3,3,3,3,4),(-22.6985303271799,-22.6163542019208,
-21.6330344540112,-20.6497147061016,-19.666394958192,-18.6830752102824,
-17.6997554623728,-16.7164357144632,-16.4153450200003),.UNSPECIFIED.);
#2153=B_SPLINE_CURVE_WITH_KNOTS('',3,(#31582,#31583,#31584,#31585,#31586,
#31587,#31588,#31589,#31590,#31591,#31592,#31593,#31594,#31595,#31596,#31597,
#31598,#31599,#31600,#31601,#31602,#31603),.UNSPECIFIED.,.F.,.F.,(4,3,3,
3,3,3,3,4),(13.8759337553363,14.749796218644,15.7331159665536,16.7164357144632,
17.6997554623728,18.6830752102824,19.666394958192,20.1591190625159),
 .UNSPECIFIED.);
#2154=B_SPLINE_CURVE_WITH_KNOTS('',3,(#31604,#31605,#31606,#31607,#31608,
#31609,#31610,#31611,#31612,#31613,#31614,#31615,#31616,#31617,#31618,#31619,
#31620,#31621,#31622,#31623,#31624,#31625),.UNSPECIFIED.,.F.,.F.,(4,3,3,
3,3,3,3,4),(-16.4153450200003,-15.7331159665536,-14.749796218644,-13.7664764707344,
-12.7831567228248,-11.7998369749152,-10.8165172270056,-10.1321597128207),
 .UNSPECIFIED.);
#2155=B_SPLINE_CURVE_WITH_KNOTS('',3,(#31631,#31632,#31633,#31634,#31635,
#31636,#31637,#31638,#31639,#31640,#31641,#31642,#31643),.UNSPECIFIED.,
 .F.,.F.,(4,3,3,3,4),(-3.84897440564114,-2.9499592437288,-1.9666394958192,
-0.983319747909601,0.),.UNSPECIFIED.);
#2156=B_SPLINE_CURVE_WITH_KNOTS('',3,(#31646,#31647,#31648,#31649,#31650,
#31651,#31652,#31653,#31654,#31655,#31656,#31657,#31658,#31659,#31660,#31661,
#31662,#31663,#31664),.UNSPECIFIED.,.F.,.F.,(4,3,3,3,3,3,4),(2.01694489302844,
2.9499592437288,3.9332789916384,4.916598739548,5.8999184874576,6.8832382353672,
7.59274844815668),.UNSPECIFIED.);
#2157=B_SPLINE_CURVE_WITH_KNOTS('',3,(#31670,#31671,#31672,#31673,#31674,
#31675,#31676,#31677),.UNSPECIFIED.,.F.,.F.,(4,1,1,1,1,4),(40.8407044966673,
41.3585812995958,42.3419010475054,43.325220795415,44.3085405433246,45.2918602912342),
 .UNSPECIFIED.);
#2158=B_SPLINE_CURVE_WITH_KNOTS('',3,(#31680,#31681,#31682,#31683,#31684,
#31685,#31686,#31687,#31688),.UNSPECIFIED.,.F.,.F.,(4,1,1,1,1,1,4),(40.8407044966673,
40.948033320531,41.9313530684406,42.9146728163502,43.8979925642598,44.8813123121694,
45.8143266628698),.UNSPECIFIED.);
#2159=B_SPLINE_CURVE_WITH_KNOTS('',3,(#31693,#31694,#31695,#31696,#31697,
#31698,#31699,#31700,#31701,#31702),.UNSPECIFIED.,.F.,.F.,(4,1,1,1,1,1,
1,4),(34.5575191894877,35.4586628121382,36.4419825600478,37.4253023079574,
38.408622055867,39.3919418037766,40.3752615516862,40.8407044966673),
 .UNSPECIFIED.);
#2160=B_SPLINE_CURVE_WITH_KNOTS('',3,(#31703,#31704,#31705,#31706,#31707,
#31708,#31709,#31710,#31711,#31712),.UNSPECIFIED.,.F.,.F.,(4,1,1,1,1,1,
1,4),(34.5575191894877,35.0481148330734,36.031434580983,37.0147543288926,
37.9980740768022,38.9813938247118,39.9647135726214,40.8407044966673),
 .UNSPECIFIED.);
#2161=B_SPLINE_CURVE_WITH_KNOTS('',3,(#31717,#31718,#31719,#31720,#31721,
#31722,#31723,#31724,#31725,#31726,#31727),.UNSPECIFIED.,.F.,.F.,(4,1,1,
1,1,1,1,1,4),(28.2743338823081,28.575424576771,29.5587443246806,30.5420640725902,
31.5253838204998,32.5087035684094,33.492023316319,34.4753430642286,34.5575191894877),
 .UNSPECIFIED.);
#2162=B_SPLINE_CURVE_WITH_KNOTS('',3,(#31728,#31729,#31730,#31731,#31732,
#31733,#31734,#31735,#31736,#31737),.UNSPECIFIED.,.F.,.F.,(4,1,1,1,1,1,
1,4),(28.2743338823081,29.1481963456159,30.1315160935254,31.114835841435,
32.0981555893446,33.0814753372542,34.0647950851639,34.5575191894877),
 .UNSPECIFIED.);
#2163=B_SPLINE_CURVE_WITH_KNOTS('',3,(#31742,#31743,#31744,#31745,#31746,
#31747,#31748,#31749,#31750,#31751),.UNSPECIFIED.,.F.,.F.,(4,1,1,1,1,1,
1,4),(21.9911485751285,22.6755060893134,23.658825837223,24.6421455851326,
25.6254653330422,26.6087850809518,27.5921048288614,28.2743338823081),
 .UNSPECIFIED.);
#2164=B_SPLINE_CURVE_WITH_KNOTS('',3,(#31752,#31753,#31754,#31755,#31756,
#31757,#31758,#31759,#31760,#31761,#31762),.UNSPECIFIED.,.F.,.F.,(4,1,1,
1,1,1,1,1,4),(21.9911485751285,22.2649581102487,23.2482778581583,24.2315976060679,
25.2149173539775,26.1982371018871,27.1815568497966,28.1648765977063,28.2743338823081),
 .UNSPECIFIED.);
#2165=B_SPLINE_CURVE_WITH_KNOTS('',3,(#31768,#31769,#31770,#31771,#31772),
 .UNSPECIFIED.,.F.,.F.,(4,1,4),(14.3984001269719,15.3817198748815,15.7079632679489),
 .UNSPECIFIED.);
#2166=B_SPLINE_CURVE_WITH_KNOTS('',3,(#31775,#31776,#31777,#31778,#31779),
 .UNSPECIFIED.,.F.,.F.,(4,1,4),(13.8759337553363,14.8089481060366,15.7079632679489),
 .UNSPECIFIED.);
#2167=B_SPLINE_CURVE_WITH_KNOTS('',3,(#31781,#31782,#31783,#31784,#31785,
#31786,#31787,#31788,#31789,#31790,#31791),.UNSPECIFIED.,.F.,.F.,(4,1,1,
1,1,1,1,1,4),(15.7079632679489,15.7922678539462,16.7755876018558,17.7589073497654,
18.742227097675,19.7255468455846,20.7088665934942,21.6921863414038,21.9911485751285),
 .UNSPECIFIED.);
#2168=B_SPLINE_CURVE_WITH_KNOTS('',3,(#31792,#31793,#31794,#31795,#31796,
#31797,#31798,#31799,#31800,#31801),.UNSPECIFIED.,.F.,.F.,(4,1,1,1,1,1,
1,4),(15.7079632679489,16.3650396227911,17.3483593707007,18.3316791186103,
19.3149988665199,20.2983186144295,21.2816383623391,21.9911485751285),
 .UNSPECIFIED.);
#2169=B_SPLINE_CURVE_WITH_KNOTS('',3,(#31950,#31951,#31952,#31953,#31954,
#31955,#31956,#31957,#31958,#31959,#31960,#31961,#31962,#31963,#31964,#31965,
#31966,#31967,#31968,#31969,#31970,#31971,#31972,#31973,#31974,#31975,#31976,
#31977,#31978,#31979,#31980,#31981,#31982,#31983,#31984,#31985,#31986,#31987,
#31988,#31989,#31990,#31991,#31992,#31993,#31994,#31995,#31996,#31997,#31998,
#31999,#32000,#32001,#32002,#32003,#32004,#32005,#32006,#32007,#32008,#32009,
#32010,#32011,#32012,#32013,#32014,#32015,#32016,#32017,#32018,#32019,#32020,
#32021,#32022,#32023,#32024,#32025,#32026,#32027,#32028,#32029,#32030,#32031,
#32032,#32033,#32034,#32035,#32036,#32037),.UNSPECIFIED.,.F.,.F.,(4,3,3,
3,3,3,3,3,3,3,3,3,3,3,3,3,3,3,3,3,3,3,3,3,3,3,3,3,3,4),(0.,0.0297382846428454,
0.0601255889259488,0.0890332382811597,0.114327431466969,0.120650702355347,
0.150403564921709,0.179988720829457,0.207838236564002,0.229395399392172,
0.23393415783729,0.262660470802463,0.291386783767636,0.320322059900051,
0.335078154046361,0.340193241308639,0.344573678198122,0.372678327643481,
0.400795960862634,0.428486852199556,0.439053852931727,0.445278633015735,
0.450309834423539,0.477267903159324,0.497055818929743,0.50468887016549,
0.511949053885254,0.537905662994819,0.556419566241001,0.569248610399422),
 .UNSPECIFIED.);
#2170=B_SPLINE_CURVE_WITH_KNOTS('',3,(#32038,#32039,#32040,#32041,#32042,
#32043,#32044,#32045,#32046,#32047,#32048,#32049,#32050,#32051,#32052,#32053,
#32054,#32055,#32056,#32057,#32058,#32059,#32060,#32061,#32062,#32063,#32064,
#32065,#32066,#32067,#32068,#32069,#32070,#32071,#32072,#32073,#32074,#32075,
#32076,#32077,#32078,#32079,#32080,#32081,#32082,#32083,#32084,#32085,#32086,
#32087,#32088,#32089,#32090,#32091,#32092,#32093,#32094,#32095,#32096,#32097,
#32098,#32099,#32100,#32101,#32102,#32103,#32104,#32105,#32106,#32107,#32108,
#32109,#32110,#32111,#32112,#32113,#32114,#32115,#32116,#32117,#32118,#32119,
#32120,#32121,#32122,#32123,#32124,#32125,#32126,#32127,#32128,#32129,#32130,
#32131),.UNSPECIFIED.,.F.,.F.,(4,3,3,3,3,3,3,3,3,3,3,3,3,3,3,3,3,3,3,3,
3,3,3,3,3,3,3,3,3,3,3,4),(0.,0.0253795104813928,0.0514287956022284,0.0778538073776754,
0.0899945430700518,0.0969018068642677,0.102642146791298,0.129947872947979,
0.157699027910297,0.183981493384174,0.195665040532001,0.201809460807294,
0.206412496951858,0.235040986639171,0.262828889805804,0.290686253909393,
0.306981212992593,0.31132393091396,0.315703998135388,0.34516669827354,0.374337762706802,
0.403793893800065,0.41497713906407,0.422789593408606,0.427299404513114,
0.458325953194986,0.48159586470639,0.493906250475823,0.500072154367986,
0.530578895950629,0.551405599240602,0.566847306048089),.UNSPECIFIED.);
#2171=B_SPLINE_CURVE_WITH_KNOTS('',3,(#32132,#32133,#32134,#32135,#32136,
#32137,#32138,#32139,#32140,#32141,#32142,#32143,#32144,#32145,#32146,#32147,
#32148,#32149,#32150,#32151,#32152,#32153,#32154,#32155,#32156),
 .UNSPECIFIED.,.F.,.F.,(4,3,3,3,3,3,3,3,4),(-10.1321597128207,-9.833197479096,
-8.8498777311864,-7.8665579832768,-6.8832382353672,-5.8999184874576,-4.916598739548,
-3.9332789916384,-3.84897440564114),.UNSPECIFIED.);
#2172=B_SPLINE_CURVE_WITH_KNOTS('',3,(#32305,#32306,#32307,#32308,#32309,
#32310,#32311,#32312,#32313,#32314,#32315,#32316,#32317,#32318,#32319,#32320,
#32321,#32322,#32323,#32324,#32325,#32326,#32327,#32328,#32329,#32330,#32331,
#32332,#32333,#32334,#32335,#32336,#32337,#32338,#32339,#32340,#32341,#32342,
#32343,#32344,#32345,#32346,#32347,#32348,#32349,#32350,#32351,#32352,#32353,
#32354,#32355,#32356,#32357,#32358,#32359,#32360,#32361,#32362,#32363,#32364,
#32365,#32366,#32367,#32368,#32369,#32370,#32371,#32372,#32373,#32374,#32375,
#32376,#32377,#32378,#32379,#32380,#32381,#32382,#32383,#32384,#32385,#32386,
#32387,#32388,#32389,#32390,#32391,#32392,#32393,#32394,#32395,#32396,#32397,
#32398),.UNSPECIFIED.,.F.,.F.,(4,3,3,3,3,3,3,3,3,3,3,3,3,3,3,3,3,3,3,3,
3,3,3,3,3,3,3,3,3,3,3,4),(0.,0.0253795895352918,0.0514289454719094,0.0778539385136474,
0.0899945864079409,0.0969018005134045,0.102642148135923,0.129947928392544,
0.157699108353734,0.183981553716754,0.195665088727664,0.201809360898104,
0.206412522774552,0.235041003890312,0.262828889805813,0.290686211240011,
0.306981172990049,0.311324022663455,0.315704013189775,0.345166711446132,
0.374337752779982,0.403793879145986,0.414977105191051,0.422789478907973,
0.427299173709167,0.458325780092032,0.481595734879181,0.493906100937864,
0.500072114794957,0.530578856744846,0.551405599240626,0.566847306048098),
 .UNSPECIFIED.);
#2173=B_SPLINE_CURVE_WITH_KNOTS('',3,(#32399,#32400,#32401,#32402,#32403,
#32404,#32405,#32406,#32407,#32408,#32409,#32410,#32411,#32412,#32413,#32414,
#32415,#32416,#32417,#32418,#32419,#32420,#32421,#32422,#32423),
 .UNSPECIFIED.,.F.,.F.,(4,3,3,3,3,3,3,3,4),(7.59274844815668,7.8665579832768,
8.84987773118639,9.833197479096,10.8165172270056,11.7998369749152,12.7831567228248,
13.7664764707344,13.8759337553363),.UNSPECIFIED.);
#2174=B_SPLINE_CURVE_WITH_KNOTS('',3,(#32424,#32425,#32426,#32427,#32428,
#32429,#32430,#32431,#32432,#32433,#32434,#32435,#32436,#32437,#32438,#32439,
#32440,#32441,#32442,#32443,#32444,#32445,#32446,#32447,#32448,#32449,#32450,
#32451,#32452,#32453,#32454,#32455,#32456,#32457,#32458,#32459,#32460,#32461,
#32462,#32463,#32464,#32465,#32466,#32467,#32468,#32469,#32470,#32471,#32472,
#32473,#32474,#32475,#32476,#32477,#32478,#32479,#32480,#32481,#32482,#32483,
#32484,#32485,#32486,#32487,#32488,#32489,#32490,#32491,#32492,#32493,#32494,
#32495,#32496,#32497,#32498,#32499,#32500,#32501,#32502,#32503,#32504,#32505,
#32506,#32507,#32508,#32509,#32510,#32511),.UNSPECIFIED.,.F.,.F.,(4,3,3,
3,3,3,3,3,3,3,3,3,3,3,3,3,3,3,3,3,3,3,3,3,3,3,3,3,3,4),(0.,0.0297383502225738,
0.0601256857797807,0.0890333230282637,0.114327505620686,0.120650688809437,
0.150403550371837,0.179988686667598,0.207838210942609,0.229395337968592,
0.23393415684471,0.262660470306177,0.291386783767645,0.32032206170552,0.335078155738989,
0.340193228824031,0.344573672707814,0.372678323504497,0.400795954000531,
0.428486824889168,0.439053762328703,0.445278745781163,0.450309838937034,
0.477267882086698,0.497055803125278,0.504688833353528,0.511949049757023,
0.537905617573998,0.556419566241016,0.569248610399434),.UNSPECIFIED.);
#2175=LINE('',#11354,#2721);
#2176=LINE('',#11363,#2722);
#2177=LINE('',#11380,#2723);
#2178=LINE('',#11428,#2724);
#2179=LINE('',#11479,#2725);
#2180=LINE('',#11527,#2726);
#2181=LINE('',#11575,#2727);
#2182=LINE('',#11626,#2728);
#2183=LINE('',#11677,#2729);
#2184=LINE('',#11725,#2730);
#2185=LINE('',#11776,#2731);
#2186=LINE('',#11827,#2732);
#2187=LINE('',#11875,#2733);
#2188=LINE('',#11923,#2734);
#2189=LINE('',#11974,#2735);
#2190=LINE('',#12025,#2736);
#2191=LINE('',#12073,#2737);
#2192=LINE('',#12124,#2738);
#2193=LINE('',#12163,#2739);
#2194=LINE('',#12187,#2740);
#2195=LINE('',#12211,#2741);
#2196=LINE('',#12236,#2742);
#2197=LINE('',#12260,#2743);
#2198=LINE('',#12285,#2744);
#2199=LINE('',#12309,#2745);
#2200=LINE('',#12334,#2746);
#2201=LINE('',#12359,#2747);
#2202=LINE('',#12383,#2748);
#2203=LINE('',#12408,#2749);
#2204=LINE('',#12432,#2750);
#2205=LINE('',#12457,#2751);
#2206=LINE('',#12481,#2752);
#2207=LINE('',#12506,#2753);
#2208=LINE('',#12531,#2754);
#2209=LINE('',#12555,#2755);
#2210=LINE('',#12572,#2756);
#2211=LINE('',#12581,#2757);
#2212=LINE('',#12598,#2758);
#2213=LINE('',#12646,#2759);
#2214=LINE('',#12697,#2760);
#2215=LINE('',#12745,#2761);
#2216=LINE('',#12793,#2762);
#2217=LINE('',#12844,#2763);
#2218=LINE('',#12895,#2764);
#2219=LINE('',#12943,#2765);
#2220=LINE('',#12994,#2766);
#2221=LINE('',#13045,#2767);
#2222=LINE('',#13093,#2768);
#2223=LINE('',#13141,#2769);
#2224=LINE('',#13192,#2770);
#2225=LINE('',#13243,#2771);
#2226=LINE('',#13291,#2772);
#2227=LINE('',#13342,#2773);
#2228=LINE('',#13381,#2774);
#2229=LINE('',#13405,#2775);
#2230=LINE('',#13429,#2776);
#2231=LINE('',#13454,#2777);
#2232=LINE('',#13478,#2778);
#2233=LINE('',#13503,#2779);
#2234=LINE('',#13527,#2780);
#2235=LINE('',#13552,#2781);
#2236=LINE('',#13577,#2782);
#2237=LINE('',#13601,#2783);
#2238=LINE('',#13626,#2784);
#2239=LINE('',#13650,#2785);
#2240=LINE('',#13675,#2786);
#2241=LINE('',#13699,#2787);
#2242=LINE('',#13724,#2788);
#2243=LINE('',#13749,#2789);
#2244=LINE('',#13773,#2790);
#2245=LINE('',#13790,#2791);
#2246=LINE('',#13799,#2792);
#2247=LINE('',#13816,#2793);
#2248=LINE('',#13864,#2794);
#2249=LINE('',#13915,#2795);
#2250=LINE('',#13963,#2796);
#2251=LINE('',#14011,#2797);
#2252=LINE('',#14062,#2798);
#2253=LINE('',#14113,#2799);
#2254=LINE('',#14161,#2800);
#2255=LINE('',#14212,#2801);
#2256=LINE('',#14263,#2802);
#2257=LINE('',#14311,#2803);
#2258=LINE('',#14359,#2804);
#2259=LINE('',#14410,#2805);
#2260=LINE('',#14461,#2806);
#2261=LINE('',#14509,#2807);
#2262=LINE('',#14560,#2808);
#2263=LINE('',#14599,#2809);
#2264=LINE('',#14623,#2810);
#2265=LINE('',#14647,#2811);
#2266=LINE('',#14672,#2812);
#2267=LINE('',#14696,#2813);
#2268=LINE('',#14721,#2814);
#2269=LINE('',#14745,#2815);
#2270=LINE('',#14770,#2816);
#2271=LINE('',#14795,#2817);
#2272=LINE('',#14819,#2818);
#2273=LINE('',#14844,#2819);
#2274=LINE('',#14868,#2820);
#2275=LINE('',#14893,#2821);
#2276=LINE('',#14917,#2822);
#2277=LINE('',#14942,#2823);
#2278=LINE('',#14967,#2824);
#2279=LINE('',#14991,#2825);
#2280=LINE('',#15008,#2826);
#2281=LINE('',#15017,#2827);
#2282=LINE('',#15034,#2828);
#2283=LINE('',#15082,#2829);
#2284=LINE('',#15133,#2830);
#2285=LINE('',#15181,#2831);
#2286=LINE('',#15229,#2832);
#2287=LINE('',#15280,#2833);
#2288=LINE('',#15331,#2834);
#2289=LINE('',#15379,#2835);
#2290=LINE('',#15430,#2836);
#2291=LINE('',#15481,#2837);
#2292=LINE('',#15529,#2838);
#2293=LINE('',#15577,#2839);
#2294=LINE('',#15628,#2840);
#2295=LINE('',#15679,#2841);
#2296=LINE('',#15727,#2842);
#2297=LINE('',#15778,#2843);
#2298=LINE('',#15817,#2844);
#2299=LINE('',#15841,#2845);
#2300=LINE('',#15865,#2846);
#2301=LINE('',#15890,#2847);
#2302=LINE('',#15914,#2848);
#2303=LINE('',#15939,#2849);
#2304=LINE('',#15963,#2850);
#2305=LINE('',#15988,#2851);
#2306=LINE('',#16013,#2852);
#2307=LINE('',#16037,#2853);
#2308=LINE('',#16062,#2854);
#2309=LINE('',#16086,#2855);
#2310=LINE('',#16111,#2856);
#2311=LINE('',#16135,#2857);
#2312=LINE('',#16160,#2858);
#2313=LINE('',#16185,#2859);
#2314=LINE('',#16209,#2860);
#2315=LINE('',#21590,#2861);
#2316=LINE('',#21592,#2862);
#2317=LINE('',#21594,#2863);
#2318=LINE('',#21595,#2864);
#2319=LINE('',#21598,#2865);
#2320=LINE('',#21600,#2866);
#2321=LINE('',#21601,#2867);
#2322=LINE('',#21604,#2868);
#2323=LINE('',#21606,#2869);
#2324=LINE('',#21607,#2870);
#2325=LINE('',#21609,#2871);
#2326=LINE('',#21610,#2872);
#2327=LINE('',#21614,#2873);
#2328=LINE('',#21616,#2874);
#2329=LINE('',#21618,#2875);
#2330=LINE('',#21619,#2876);
#2331=LINE('',#21622,#2877);
#2332=LINE('',#21624,#2878);
#2333=LINE('',#21625,#2879);
#2334=LINE('',#21628,#2880);
#2335=LINE('',#21630,#2881);
#2336=LINE('',#21631,#2882);
#2337=LINE('',#21633,#2883);
#2338=LINE('',#21634,#2884);
#2339=LINE('',#21642,#2885);
#2340=LINE('',#21648,#2886);
#2341=LINE('',#21654,#2887);
#2342=LINE('',#21660,#2888);
#2343=LINE('',#21666,#2889);
#2344=LINE('',#21671,#2890);
#2345=LINE('',#21673,#2891);
#2346=LINE('',#21675,#2892);
#2347=LINE('',#21676,#2893);
#2348=LINE('',#21679,#2894);
#2349=LINE('',#21681,#2895);
#2350=LINE('',#21682,#2896);
#2351=LINE('',#21685,#2897);
#2352=LINE('',#21687,#2898);
#2353=LINE('',#21688,#2899);
#2354=LINE('',#21690,#2900);
#2355=LINE('',#21691,#2901);
#2356=LINE('',#21698,#2902);
#2357=LINE('',#21700,#2903);
#2358=LINE('',#21702,#2904);
#2359=LINE('',#21703,#2905);
#2360=LINE('',#21706,#2906);
#2361=LINE('',#21708,#2907);
#2362=LINE('',#21709,#2908);
#2363=LINE('',#21712,#2909);
#2364=LINE('',#21714,#2910);
#2365=LINE('',#21715,#2911);
#2366=LINE('',#21717,#2912);
#2367=LINE('',#21718,#2913);
#2368=LINE('',#21722,#2914);
#2369=LINE('',#21724,#2915);
#2370=LINE('',#21726,#2916);
#2371=LINE('',#21727,#2917);
#2372=LINE('',#21730,#2918);
#2373=LINE('',#21732,#2919);
#2374=LINE('',#21733,#2920);
#2375=LINE('',#21736,#2921);
#2376=LINE('',#21738,#2922);
#2377=LINE('',#21739,#2923);
#2378=LINE('',#21741,#2924);
#2379=LINE('',#21742,#2925);
#2380=LINE('',#21749,#2926);
#2381=LINE('',#21778,#2927);
#2382=LINE('',#21805,#2928);
#2383=LINE('',#21856,#2929);
#2384=LINE('',#21904,#2930);
#2385=LINE('',#21955,#2931);
#2386=LINE('',#22006,#2932);
#2387=LINE('',#22054,#2933);
#2388=LINE('',#22102,#2934);
#2389=LINE('',#22153,#2935);
#2390=LINE('',#22201,#2936);
#2391=LINE('',#22249,#2937);
#2392=LINE('',#22300,#2938);
#2393=LINE('',#22351,#2939);
#2394=LINE('',#22399,#2940);
#2395=LINE('',#22450,#2941);
#2396=LINE('',#22489,#2942);
#2397=LINE('',#22509,#2943);
#2398=LINE('',#22533,#2944);
#2399=LINE('',#22558,#2945);
#2400=LINE('',#22583,#2946);
#2401=LINE('',#22607,#2947);
#2402=LINE('',#22632,#2948);
#2403=LINE('',#22656,#2949);
#2404=LINE('',#22681,#2950);
#2405=LINE('',#22706,#2951);
#2406=LINE('',#22730,#2952);
#2407=LINE('',#22755,#2953);
#2408=LINE('',#22779,#2954);
#2409=LINE('',#22804,#2955);
#2410=LINE('',#22829,#2956);
#2411=LINE('',#22853,#2957);
#2412=LINE('',#24114,#2958);
#2413=LINE('',#24116,#2959);
#2414=LINE('',#24118,#2960);
#2415=LINE('',#24119,#2961);
#2416=LINE('',#24122,#2962);
#2417=LINE('',#24124,#2963);
#2418=LINE('',#24125,#2964);
#2419=LINE('',#24128,#2965);
#2420=LINE('',#24130,#2966);
#2421=LINE('',#24131,#2967);
#2422=LINE('',#24133,#2968);
#2423=LINE('',#24134,#2969);
#2424=LINE('',#24140,#2970);
#2425=LINE('',#24151,#2971);
#2426=LINE('',#24155,#2972);
#2427=LINE('',#24157,#2973);
#2428=LINE('',#24159,#2974);
#2429=LINE('',#24160,#2975);
#2430=LINE('',#24163,#2976);
#2431=LINE('',#24165,#2977);
#2432=LINE('',#24166,#2978);
#2433=LINE('',#24169,#2979);
#2434=LINE('',#24171,#2980);
#2435=LINE('',#24172,#2981);
#2436=LINE('',#24175,#2982);
#2437=LINE('',#24177,#2983);
#2438=LINE('',#24178,#2984);
#2439=LINE('',#24181,#2985);
#2440=LINE('',#24183,#2986);
#2441=LINE('',#24184,#2987);
#2442=LINE('',#24186,#2988);
#2443=LINE('',#24187,#2989);
#2444=LINE('',#24196,#2990);
#2445=LINE('',#24200,#2991);
#2446=LINE('',#24206,#2992);
#2447=LINE('',#24208,#2993);
#2448=LINE('',#24210,#2994);
#2449=LINE('',#24211,#2995);
#2450=LINE('',#24214,#2996);
#2451=LINE('',#24216,#2997);
#2452=LINE('',#24217,#2998);
#2453=LINE('',#24220,#2999);
#2454=LINE('',#24222,#3000);
#2455=LINE('',#24223,#3001);
#2456=LINE('',#24226,#3002);
#2457=LINE('',#24228,#3003);
#2458=LINE('',#24229,#3004);
#2459=LINE('',#24232,#3005);
#2460=LINE('',#24234,#3006);
#2461=LINE('',#24235,#3007);
#2462=LINE('',#24237,#3008);
#2463=LINE('',#24238,#3009);
#2464=LINE('',#24242,#3010);
#2465=LINE('',#24244,#3011);
#2466=LINE('',#24246,#3012);
#2467=LINE('',#24247,#3013);
#2468=LINE('',#24250,#3014);
#2469=LINE('',#24252,#3015);
#2470=LINE('',#24253,#3016);
#2471=LINE('',#24256,#3017);
#2472=LINE('',#24258,#3018);
#2473=LINE('',#24259,#3019);
#2474=LINE('',#24261,#3020);
#2475=LINE('',#24262,#3021);
#2476=LINE('',#24270,#3022);
#2477=LINE('',#24276,#3023);
#2478=LINE('',#24284,#3024);
#2479=LINE('',#24286,#3025);
#2480=LINE('',#24288,#3026);
#2481=LINE('',#24289,#3027);
#2482=LINE('',#24293,#3028);
#2483=LINE('',#24295,#3029);
#2484=LINE('',#24297,#3030);
#2485=LINE('',#24298,#3031);
#2486=LINE('',#24312,#3032);
#2487=LINE('',#24318,#3033);
#2488=LINE('',#24326,#3034);
#2489=LINE('',#24350,#3035);
#2490=LINE('',#24398,#3036);
#2491=LINE('',#24446,#3037);
#2492=LINE('',#24497,#3038);
#2493=LINE('',#24548,#3039);
#2494=LINE('',#24596,#3040);
#2495=LINE('',#24644,#3041);
#2496=LINE('',#24698,#3042);
#2497=LINE('',#24746,#3043);
#2498=LINE('',#24794,#3044);
#2499=LINE('',#24819,#3045);
#2500=LINE('',#24844,#3046);
#2501=LINE('',#24868,#3047);
#2502=LINE('',#24893,#3048);
#2503=LINE('',#24918,#3049);
#2504=LINE('',#24942,#3050);
#2505=LINE('',#24966,#3051);
#2506=LINE('',#24992,#3052);
#2507=LINE('',#25016,#3053);
#2508=LINE('',#25334,#3054);
#2509=LINE('',#26137,#3055);
#2510=LINE('',#26139,#3056);
#2511=LINE('',#26141,#3057);
#2512=LINE('',#26142,#3058);
#2513=LINE('',#26145,#3059);
#2514=LINE('',#26147,#3060);
#2515=LINE('',#26148,#3061);
#2516=LINE('',#26151,#3062);
#2517=LINE('',#26153,#3063);
#2518=LINE('',#26154,#3064);
#2519=LINE('',#26157,#3065);
#2520=LINE('',#26159,#3066);
#2521=LINE('',#26160,#3067);
#2522=LINE('',#26163,#3068);
#2523=LINE('',#26165,#3069);
#2524=LINE('',#26166,#3070);
#2525=LINE('',#26168,#3071);
#2526=LINE('',#26169,#3072);
#2527=LINE('',#26176,#3073);
#2528=LINE('',#26184,#3074);
#2529=LINE('',#26186,#3075);
#2530=LINE('',#26188,#3076);
#2531=LINE('',#26189,#3077);
#2532=LINE('',#26192,#3078);
#2533=LINE('',#26194,#3079);
#2534=LINE('',#26196,#3080);
#2535=LINE('',#26198,#3081);
#2536=LINE('',#26200,#3082);
#2537=LINE('',#26202,#3083);
#2538=LINE('',#26203,#3084);
#2539=LINE('',#26210,#3085);
#2540=LINE('',#26214,#3086);
#2541=LINE('',#26219,#3087);
#2542=LINE('',#26226,#3088);
#2543=LINE('',#26229,#3089);
#2544=LINE('',#26232,#3090);
#2545=LINE('',#26238,#3091);
#2546=LINE('',#26242,#3092);
#2547=LINE('',#26246,#3093);
#2548=LINE('',#26247,#3094);
#2549=LINE('',#26250,#3095);
#2550=LINE('',#26251,#3096);
#2551=LINE('',#26253,#3097);
#2552=LINE('',#26260,#3098);
#2553=LINE('',#26271,#3099);
#2554=LINE('',#26279,#3100);
#2555=LINE('',#26283,#3101);
#2556=LINE('',#26289,#3102);
#2557=LINE('',#26291,#3103);
#2558=LINE('',#26293,#3104);
#2559=LINE('',#26294,#3105);
#2560=LINE('',#26298,#3106);
#2561=LINE('',#26300,#3107);
#2562=LINE('',#26302,#3108);
#2563=LINE('',#26303,#3109);
#2564=LINE('',#26316,#3110);
#2565=LINE('',#26318,#3111);
#2566=LINE('',#26320,#3112);
#2567=LINE('',#26321,#3113);
#2568=LINE('',#26325,#3114);
#2569=LINE('',#26327,#3115);
#2570=LINE('',#26329,#3116);
#2571=LINE('',#26330,#3117);
#2572=LINE('',#26333,#3118);
#2573=LINE('',#26335,#3119);
#2574=LINE('',#26336,#3120);
#2575=LINE('',#26338,#3121);
#2576=LINE('',#26340,#3122);
#2577=LINE('',#26341,#3123);
#2578=LINE('',#26348,#3124);
#2579=LINE('',#26349,#3125);
#2580=LINE('',#26353,#3126);
#2581=LINE('',#26357,#3127);
#2582=LINE('',#26361,#3128);
#2583=LINE('',#26366,#3129);
#2584=LINE('',#26370,#3130);
#2585=LINE('',#26373,#3131);
#2586=LINE('',#26376,#3132);
#2587=LINE('',#26377,#3133);
#2588=LINE('',#26379,#3134);
#2589=LINE('',#26386,#3135);
#2590=LINE('',#26392,#3136);
#2591=LINE('',#26400,#3137);
#2592=LINE('',#26424,#3138);
#2593=LINE('',#26472,#3139);
#2594=LINE('',#26520,#3140);
#2595=LINE('',#26574,#3141);
#2596=LINE('',#26622,#3142);
#2597=LINE('',#26670,#3143);
#2598=LINE('',#26724,#3144);
#2599=LINE('',#26772,#3145);
#2600=LINE('',#26820,#3146);
#2601=LINE('',#26868,#3147);
#2602=LINE('',#26922,#3148);
#2603=LINE('',#26970,#3149);
#2604=LINE('',#27018,#3150);
#2605=LINE('',#27072,#3151);
#2606=LINE('',#27120,#3152);
#2607=LINE('',#27168,#3153);
#2608=LINE('',#27222,#3154);
#2609=LINE('',#27270,#3155);
#2610=LINE('',#27318,#3156);
#2611=LINE('',#27343,#3157);
#2612=LINE('',#27368,#3158);
#2613=LINE('',#27392,#3159);
#2614=LINE('',#27417,#3160);
#2615=LINE('',#27442,#3161);
#2616=LINE('',#27466,#3162);
#2617=LINE('',#27491,#3163);
#2618=LINE('',#27516,#3164);
#2619=LINE('',#27540,#3165);
#2620=LINE('',#27565,#3166);
#2621=LINE('',#27590,#3167);
#2622=LINE('',#27614,#3168);
#2623=LINE('',#27638,#3169);
#2624=LINE('',#27663,#3170);
#2625=LINE('',#27688,#3171);
#2626=LINE('',#27712,#3172);
#2627=LINE('',#27737,#3173);
#2628=LINE('',#27762,#3174);
#2629=LINE('',#28101,#3175);
#2630=LINE('',#29375,#3176);
#2631=LINE('',#29377,#3177);
#2632=LINE('',#29379,#3178);
#2633=LINE('',#29380,#3179);
#2634=LINE('',#29383,#3180);
#2635=LINE('',#29385,#3181);
#2636=LINE('',#29386,#3182);
#2637=LINE('',#29389,#3183);
#2638=LINE('',#29391,#3184);
#2639=LINE('',#29392,#3185);
#2640=LINE('',#29395,#3186);
#2641=LINE('',#29397,#3187);
#2642=LINE('',#29398,#3188);
#2643=LINE('',#29401,#3189);
#2644=LINE('',#29403,#3190);
#2645=LINE('',#29404,#3191);
#2646=LINE('',#29406,#3192);
#2647=LINE('',#29407,#3193);
#2648=LINE('',#29414,#3194);
#2649=LINE('',#29422,#3195);
#2650=LINE('',#29446,#3196);
#2651=LINE('',#29494,#3197);
#2652=LINE('',#29542,#3198);
#2653=LINE('',#29596,#3199);
#2654=LINE('',#29644,#3200);
#2655=LINE('',#29692,#3201);
#2656=LINE('',#29746,#3202);
#2657=LINE('',#29794,#3203);
#2658=LINE('',#29845,#3204);
#2659=LINE('',#29896,#3205);
#2660=LINE('',#29944,#3206);
#2661=LINE('',#29969,#3207);
#2662=LINE('',#29994,#3208);
#2663=LINE('',#30018,#3209);
#2664=LINE('',#30044,#3210);
#2665=LINE('',#30068,#3211);
#2666=LINE('',#30093,#3212);
#2667=LINE('',#30118,#3213);
#2668=LINE('',#30142,#3214);
#2669=LINE('',#30167,#3215);
#2670=LINE('',#30192,#3216);
#2671=LINE('',#30528,#3217);
#2672=LINE('',#31396,#3218);
#2673=LINE('',#31398,#3219);
#2674=LINE('',#31400,#3220);
#2675=LINE('',#31401,#3221);
#2676=LINE('',#31404,#3222);
#2677=LINE('',#31406,#3223);
#2678=LINE('',#31407,#3224);
#2679=LINE('',#31410,#3225);
#2680=LINE('',#31412,#3226);
#2681=LINE('',#31413,#3227);
#2682=LINE('',#31416,#3228);
#2683=LINE('',#31418,#3229);
#2684=LINE('',#31419,#3230);
#2685=LINE('',#31422,#3231);
#2686=LINE('',#31424,#3232);
#2687=LINE('',#31425,#3233);
#2688=LINE('',#31427,#3234);
#2689=LINE('',#31428,#3235);
#2690=LINE('',#31435,#3236);
#2691=LINE('',#31444,#3237);
#2692=LINE('',#31450,#3238);
#2693=LINE('',#31458,#3239);
#2694=LINE('',#31479,#3240);
#2695=LINE('',#31530,#3241);
#2696=LINE('',#31581,#3242);
#2697=LINE('',#31629,#3243);
#2698=LINE('',#31668,#3244);
#2699=LINE('',#31692,#3245);
#2700=LINE('',#31716,#3246);
#2701=LINE('',#31741,#3247);
#2702=LINE('',#31766,#3248);
#2703=LINE('',#32515,#3249);
#2704=LINE('',#32517,#3250);
#2705=LINE('',#32519,#3251);
#2706=LINE('',#32521,#3252);
#2707=LINE('',#32523,#3253);
#2708=LINE('',#32524,#3254);
#2709=LINE('',#32529,#3255);
#2710=LINE('',#32530,#3256);
#2711=LINE('',#32531,#3257);
#2712=LINE('',#32534,#3258);
#2713=LINE('',#32535,#3259);
#2714=LINE('',#32538,#3260);
#2715=LINE('',#32539,#3261);
#2716=LINE('',#32542,#3262);
#2717=LINE('',#32543,#3263);
#2718=LINE('',#32546,#3264);
#2719=LINE('',#32547,#3265);
#2720=LINE('',#32549,#3266);
#2721=VECTOR('',#9535,3.);
#2722=VECTOR('',#9538,3.);
#2723=VECTOR('',#9545,3.);
#2724=VECTOR('',#9548,3.);
#2725=VECTOR('',#9551,3.);
#2726=VECTOR('',#9554,3.);
#2727=VECTOR('',#9557,3.);
#2728=VECTOR('',#9560,3.);
#2729=VECTOR('',#9563,3.);
#2730=VECTOR('',#9566,3.);
#2731=VECTOR('',#9569,3.);
#2732=VECTOR('',#9572,3.);
#2733=VECTOR('',#9575,3.);
#2734=VECTOR('',#9578,3.);
#2735=VECTOR('',#9581,3.);
#2736=VECTOR('',#9584,3.);
#2737=VECTOR('',#9587,3.);
#2738=VECTOR('',#9590,3.);
#2739=VECTOR('',#9595,3.0735);
#2740=VECTOR('',#9600,3.0735);
#2741=VECTOR('',#9603,3.0735);
#2742=VECTOR('',#9606,3.0735);
#2743=VECTOR('',#9609,3.0735);
#2744=VECTOR('',#9612,3.0735);
#2745=VECTOR('',#9615,3.0735);
#2746=VECTOR('',#9618,3.0735);
#2747=VECTOR('',#9621,3.0735);
#2748=VECTOR('',#9624,3.0735);
#2749=VECTOR('',#9627,3.0735);
#2750=VECTOR('',#9630,3.0735);
#2751=VECTOR('',#9633,3.0735);
#2752=VECTOR('',#9636,3.0735);
#2753=VECTOR('',#9639,3.0735);
#2754=VECTOR('',#9642,3.0735);
#2755=VECTOR('',#9645,3.0735);
#2756=VECTOR('',#9650,3.);
#2757=VECTOR('',#9653,3.);
#2758=VECTOR('',#9660,3.);
#2759=VECTOR('',#9663,3.);
#2760=VECTOR('',#9666,3.);
#2761=VECTOR('',#9669,3.);
#2762=VECTOR('',#9672,3.);
#2763=VECTOR('',#9675,3.);
#2764=VECTOR('',#9678,3.);
#2765=VECTOR('',#9681,3.);
#2766=VECTOR('',#9684,3.);
#2767=VECTOR('',#9687,3.);
#2768=VECTOR('',#9690,3.);
#2769=VECTOR('',#9693,3.);
#2770=VECTOR('',#9696,3.);
#2771=VECTOR('',#9699,3.);
#2772=VECTOR('',#9702,3.);
#2773=VECTOR('',#9705,3.);
#2774=VECTOR('',#9710,3.0735);
#2775=VECTOR('',#9715,3.0735);
#2776=VECTOR('',#9718,3.0735);
#2777=VECTOR('',#9721,3.0735);
#2778=VECTOR('',#9724,3.0735);
#2779=VECTOR('',#9727,3.0735);
#2780=VECTOR('',#9730,3.0735);
#2781=VECTOR('',#9733,3.0735);
#2782=VECTOR('',#9736,3.0735);
#2783=VECTOR('',#9739,3.0735);
#2784=VECTOR('',#9742,3.0735);
#2785=VECTOR('',#9745,3.0735);
#2786=VECTOR('',#9748,3.0735);
#2787=VECTOR('',#9751,3.0735);
#2788=VECTOR('',#9754,3.0735);
#2789=VECTOR('',#9757,3.0735);
#2790=VECTOR('',#9760,3.0735);
#2791=VECTOR('',#9765,3.);
#2792=VECTOR('',#9768,3.);
#2793=VECTOR('',#9775,3.);
#2794=VECTOR('',#9778,3.);
#2795=VECTOR('',#9781,3.);
#2796=VECTOR('',#9784,3.);
#2797=VECTOR('',#9787,3.);
#2798=VECTOR('',#9790,3.);
#2799=VECTOR('',#9793,3.);
#2800=VECTOR('',#9796,3.);
#2801=VECTOR('',#9799,3.);
#2802=VECTOR('',#9802,3.);
#2803=VECTOR('',#9805,3.);
#2804=VECTOR('',#9808,3.);
#2805=VECTOR('',#9811,3.);
#2806=VECTOR('',#9814,3.);
#2807=VECTOR('',#9817,3.);
#2808=VECTOR('',#9820,3.);
#2809=VECTOR('',#9825,3.07349999999996);
#2810=VECTOR('',#9830,3.07349999999996);
#2811=VECTOR('',#9833,3.07349999999996);
#2812=VECTOR('',#9836,3.07349999999996);
#2813=VECTOR('',#9839,3.07349999999996);
#2814=VECTOR('',#9842,3.07349999999996);
#2815=VECTOR('',#9845,3.07349999999996);
#2816=VECTOR('',#9848,3.07349999999996);
#2817=VECTOR('',#9851,3.07349999999996);
#2818=VECTOR('',#9854,3.07349999999996);
#2819=VECTOR('',#9857,3.07349999999996);
#2820=VECTOR('',#9860,3.07349999999996);
#2821=VECTOR('',#9863,3.07349999999996);
#2822=VECTOR('',#9866,3.07349999999996);
#2823=VECTOR('',#9869,3.07349999999996);
#2824=VECTOR('',#9872,3.07349999999996);
#2825=VECTOR('',#9875,3.07349999999996);
#2826=VECTOR('',#9880,3.);
#2827=VECTOR('',#9883,3.);
#2828=VECTOR('',#9890,3.);
#2829=VECTOR('',#9893,3.);
#2830=VECTOR('',#9896,3.);
#2831=VECTOR('',#9899,3.);
#2832=VECTOR('',#9902,3.);
#2833=VECTOR('',#9905,3.);
#2834=VECTOR('',#9908,3.);
#2835=VECTOR('',#9911,3.);
#2836=VECTOR('',#9914,3.);
#2837=VECTOR('',#9917,3.);
#2838=VECTOR('',#9920,3.);
#2839=VECTOR('',#9923,3.);
#2840=VECTOR('',#9926,3.);
#2841=VECTOR('',#9929,3.);
#2842=VECTOR('',#9932,3.);
#2843=VECTOR('',#9935,3.);
#2844=VECTOR('',#9940,3.07350000000003);
#2845=VECTOR('',#9945,3.07350000000003);
#2846=VECTOR('',#9948,3.07350000000003);
#2847=VECTOR('',#9951,3.07350000000003);
#2848=VECTOR('',#9954,3.07350000000003);
#2849=VECTOR('',#9957,3.07350000000003);
#2850=VECTOR('',#9960,3.07350000000003);
#2851=VECTOR('',#9963,3.07350000000003);
#2852=VECTOR('',#9966,3.07350000000003);
#2853=VECTOR('',#9969,3.07350000000003);
#2854=VECTOR('',#9972,3.07350000000003);
#2855=VECTOR('',#9975,3.07350000000003);
#2856=VECTOR('',#9978,3.07350000000003);
#2857=VECTOR('',#9981,3.07350000000003);
#2858=VECTOR('',#9984,3.07350000000003);
#2859=VECTOR('',#9987,3.07350000000003);
#2860=VECTOR('',#9990,3.07350000000003);
#2861=VECTOR('',#10027,10.);
#2862=VECTOR('',#10028,10.);
#2863=VECTOR('',#10029,10.);
#2864=VECTOR('',#10030,10.);
#2865=VECTOR('',#10033,10.);
#2866=VECTOR('',#10034,10.);
#2867=VECTOR('',#10035,10.);
#2868=VECTOR('',#10038,10.);
#2869=VECTOR('',#10039,10.);
#2870=VECTOR('',#10040,10.);
#2871=VECTOR('',#10043,10.);
#2872=VECTOR('',#10044,10.);
#2873=VECTOR('',#10047,10.);
#2874=VECTOR('',#10048,10.);
#2875=VECTOR('',#10049,10.);
#2876=VECTOR('',#10050,10.);
#2877=VECTOR('',#10053,10.);
#2878=VECTOR('',#10054,10.);
#2879=VECTOR('',#10055,10.);
#2880=VECTOR('',#10058,10.);
#2881=VECTOR('',#10059,10.);
#2882=VECTOR('',#10060,10.);
#2883=VECTOR('',#10063,10.);
#2884=VECTOR('',#10064,10.);
#2885=VECTOR('',#10075,4.5);
#2886=VECTOR('',#10082,3.5);
#2887=VECTOR('',#10089,3.5);
#2888=VECTOR('',#10096,3.5);
#2889=VECTOR('',#10103,3.5);
#2890=VECTOR('',#10108,10.);
#2891=VECTOR('',#10109,10.);
#2892=VECTOR('',#10110,10.);
#2893=VECTOR('',#10111,10.);
#2894=VECTOR('',#10114,10.);
#2895=VECTOR('',#10115,10.);
#2896=VECTOR('',#10116,10.);
#2897=VECTOR('',#10119,10.);
#2898=VECTOR('',#10120,10.);
#2899=VECTOR('',#10121,10.);
#2900=VECTOR('',#10124,10.);
#2901=VECTOR('',#10125,10.);
#2902=VECTOR('',#10134,10.);
#2903=VECTOR('',#10135,10.);
#2904=VECTOR('',#10136,10.);
#2905=VECTOR('',#10137,10.);
#2906=VECTOR('',#10140,10.);
#2907=VECTOR('',#10141,10.);
#2908=VECTOR('',#10142,10.);
#2909=VECTOR('',#10145,10.);
#2910=VECTOR('',#10146,10.);
#2911=VECTOR('',#10147,10.);
#2912=VECTOR('',#10150,10.);
#2913=VECTOR('',#10151,10.);
#2914=VECTOR('',#10154,10.);
#2915=VECTOR('',#10155,10.);
#2916=VECTOR('',#10156,10.);
#2917=VECTOR('',#10157,10.);
#2918=VECTOR('',#10160,10.);
#2919=VECTOR('',#10161,10.);
#2920=VECTOR('',#10162,10.);
#2921=VECTOR('',#10165,10.);
#2922=VECTOR('',#10166,10.);
#2923=VECTOR('',#10167,10.);
#2924=VECTOR('',#10170,10.);
#2925=VECTOR('',#10171,10.);
#2926=VECTOR('',#10180,2.);
#2927=VECTOR('',#10183,2.);
#2928=VECTOR('',#10188,2.);
#2929=VECTOR('',#10191,2.);
#2930=VECTOR('',#10194,2.);
#2931=VECTOR('',#10197,2.);
#2932=VECTOR('',#10200,2.);
#2933=VECTOR('',#10203,2.);
#2934=VECTOR('',#10206,2.);
#2935=VECTOR('',#10209,2.);
#2936=VECTOR('',#10212,2.);
#2937=VECTOR('',#10215,2.);
#2938=VECTOR('',#10218,2.);
#2939=VECTOR('',#10221,2.);
#2940=VECTOR('',#10224,2.);
#2941=VECTOR('',#10227,2.);
#2942=VECTOR('',#10232,2.05475);
#2943=VECTOR('',#10237,2.05475);
#2944=VECTOR('',#10240,2.05475);
#2945=VECTOR('',#10243,2.05475);
#2946=VECTOR('',#10246,2.05475);
#2947=VECTOR('',#10249,2.05475);
#2948=VECTOR('',#10252,2.05475);
#2949=VECTOR('',#10255,2.05475);
#2950=VECTOR('',#10258,2.05475);
#2951=VECTOR('',#10261,2.05475);
#2952=VECTOR('',#10264,2.05475);
#2953=VECTOR('',#10267,2.05475);
#2954=VECTOR('',#10270,2.05475);
#2955=VECTOR('',#10273,2.05475);
#2956=VECTOR('',#10276,2.05475);
#2957=VECTOR('',#10279,2.05475);
#2958=VECTOR('',#10292,10.);
#2959=VECTOR('',#10293,10.);
#2960=VECTOR('',#10294,10.);
#2961=VECTOR('',#10295,10.);
#2962=VECTOR('',#10298,10.);
#2963=VECTOR('',#10299,10.);
#2964=VECTOR('',#10300,10.);
#2965=VECTOR('',#10303,10.);
#2966=VECTOR('',#10304,10.);
#2967=VECTOR('',#10305,10.);
#2968=VECTOR('',#10308,10.);
#2969=VECTOR('',#10309,10.);
#2970=VECTOR('',#10316,3.);
#2971=VECTOR('',#10331,4.);
#2972=VECTOR('',#10334,10.);
#2973=VECTOR('',#10335,10.);
#2974=VECTOR('',#10336,10.);
#2975=VECTOR('',#10337,10.);
#2976=VECTOR('',#10340,10.);
#2977=VECTOR('',#10341,10.);
#2978=VECTOR('',#10342,10.);
#2979=VECTOR('',#10345,10.);
#2980=VECTOR('',#10346,10.);
#2981=VECTOR('',#10347,10.);
#2982=VECTOR('',#10350,10.);
#2983=VECTOR('',#10351,10.);
#2984=VECTOR('',#10352,10.);
#2985=VECTOR('',#10355,10.);
#2986=VECTOR('',#10356,10.);
#2987=VECTOR('',#10357,10.);
#2988=VECTOR('',#10360,10.);
#2989=VECTOR('',#10361,10.);
#2990=VECTOR('',#10372,10.);
#2991=VECTOR('',#10379,4.);
#2992=VECTOR('',#10386,10.);
#2993=VECTOR('',#10387,10.);
#2994=VECTOR('',#10388,10.);
#2995=VECTOR('',#10389,10.);
#2996=VECTOR('',#10392,10.);
#2997=VECTOR('',#10393,10.);
#2998=VECTOR('',#10394,10.);
#2999=VECTOR('',#10397,10.);
#3000=VECTOR('',#10398,10.);
#3001=VECTOR('',#10399,10.);
#3002=VECTOR('',#10402,10.);
#3003=VECTOR('',#10403,10.);
#3004=VECTOR('',#10404,10.);
#3005=VECTOR('',#10407,10.);
#3006=VECTOR('',#10408,10.);
#3007=VECTOR('',#10409,10.);
#3008=VECTOR('',#10412,10.);
#3009=VECTOR('',#10413,10.);
#3010=VECTOR('',#10416,10.);
#3011=VECTOR('',#10417,10.);
#3012=VECTOR('',#10418,10.);
#3013=VECTOR('',#10419,10.);
#3014=VECTOR('',#10422,10.);
#3015=VECTOR('',#10423,10.);
#3016=VECTOR('',#10424,10.);
#3017=VECTOR('',#10427,10.);
#3018=VECTOR('',#10428,10.);
#3019=VECTOR('',#10429,10.);
#3020=VECTOR('',#10432,10.);
#3021=VECTOR('',#10433,10.);
#3022=VECTOR('',#10444,4.);
#3023=VECTOR('',#10451,8.);
#3024=VECTOR('',#10462,10.);
#3025=VECTOR('',#10463,10.);
#3026=VECTOR('',#10464,10.);
#3027=VECTOR('',#10465,10.);
#3028=VECTOR('',#10468,10.);
#3029=VECTOR('',#10469,10.);
#3030=VECTOR('',#10470,10.);
#3031=VECTOR('',#10471,10.);
#3032=VECTOR('',#10494,2.5);
#3033=VECTOR('',#10501,4.5);
#3034=VECTOR('',#10512,2.);
#3035=VECTOR('',#10517,2.);
#3036=VECTOR('',#10520,2.);
#3037=VECTOR('',#10523,2.);
#3038=VECTOR('',#10526,2.);
#3039=VECTOR('',#10529,2.);
#3040=VECTOR('',#10532,2.);
#3041=VECTOR('',#10535,2.);
#3042=VECTOR('',#10538,2.);
#3043=VECTOR('',#10541,2.);
#3044=VECTOR('',#10544,1.5555);
#3045=VECTOR('',#10549,1.5555);
#3046=VECTOR('',#10552,1.5555);
#3047=VECTOR('',#10555,1.5555);
#3048=VECTOR('',#10558,1.5555);
#3049=VECTOR('',#10561,1.5555);
#3050=VECTOR('',#10564,1.5555);
#3051=VECTOR('',#10567,1.5555);
#3052=VECTOR('',#10570,1.5555);
#3053=VECTOR('',#10573,1.5555);
#3054=VECTOR('',#10578,1.5);
#3055=VECTOR('',#10589,10.);
#3056=VECTOR('',#10590,10.);
#3057=VECTOR('',#10591,10.);
#3058=VECTOR('',#10592,10.);
#3059=VECTOR('',#10595,10.);
#3060=VECTOR('',#10596,10.);
#3061=VECTOR('',#10597,10.);
#3062=VECTOR('',#10600,10.);
#3063=VECTOR('',#10601,10.);
#3064=VECTOR('',#10602,10.);
#3065=VECTOR('',#10605,10.);
#3066=VECTOR('',#10606,10.);
#3067=VECTOR('',#10607,10.);
#3068=VECTOR('',#10610,10.);
#3069=VECTOR('',#10611,10.);
#3070=VECTOR('',#10612,10.);
#3071=VECTOR('',#10615,10.);
#3072=VECTOR('',#10616,10.);
#3073=VECTOR('',#10625,3.5);
#3074=VECTOR('',#10636,10.);
#3075=VECTOR('',#10637,10.);
#3076=VECTOR('',#10638,10.);
#3077=VECTOR('',#10639,10.);
#3078=VECTOR('',#10642,10.);
#3079=VECTOR('',#10643,10.);
#3080=VECTOR('',#10644,10.);
#3081=VECTOR('',#10645,10.);
#3082=VECTOR('',#10646,10.);
#3083=VECTOR('',#10647,10.);
#3084=VECTOR('',#10648,10.);
#3085=VECTOR('',#10655,3.5);
#3086=VECTOR('',#10660,3.5);
#3087=VECTOR('',#10665,10.);
#3088=VECTOR('',#10674,2.);
#3089=VECTOR('',#10679,10.);
#3090=VECTOR('',#10682,10.);
#3091=VECTOR('',#10689,2.);
#3092=VECTOR('',#10694,10.);
#3093=VECTOR('',#10699,10.);
#3094=VECTOR('',#10700,10.);
#3095=VECTOR('',#10703,10.);
#3096=VECTOR('',#10704,10.);
#3097=VECTOR('',#10707,10.);
#3098=VECTOR('',#10716,1.5);
#3099=VECTOR('',#10731,2.);
#3100=VECTOR('',#10740,4.);
#3101=VECTOR('',#10747,2.);
#3102=VECTOR('',#10754,10.);
#3103=VECTOR('',#10755,10.);
#3104=VECTOR('',#10756,10.);
#3105=VECTOR('',#10757,10.);
#3106=VECTOR('',#10760,10.);
#3107=VECTOR('',#10761,10.);
#3108=VECTOR('',#10762,10.);
#3109=VECTOR('',#10763,10.);
#3110=VECTOR('',#10784,10.);
#3111=VECTOR('',#10785,10.);
#3112=VECTOR('',#10786,10.);
#3113=VECTOR('',#10787,10.);
#3114=VECTOR('',#10790,10.);
#3115=VECTOR('',#10791,10.);
#3116=VECTOR('',#10792,10.);
#3117=VECTOR('',#10793,10.);
#3118=VECTOR('',#10796,10.);
#3119=VECTOR('',#10797,10.);
#3120=VECTOR('',#10798,10.);
#3121=VECTOR('',#10799,10.);
#3122=VECTOR('',#10800,10.);
#3123=VECTOR('',#10801,10.);
#3124=VECTOR('',#10808,10.);
#3125=VECTOR('',#10809,10.);
#3126=VECTOR('',#10814,3.5);
#3127=VECTOR('',#10819,3.5);
#3128=VECTOR('',#10824,10.);
#3129=VECTOR('',#10829,2.);
#3130=VECTOR('',#10834,10.);
#3131=VECTOR('',#10839,10.);
#3132=VECTOR('',#10842,10.);
#3133=VECTOR('',#10843,10.);
#3134=VECTOR('',#10846,10.);
#3135=VECTOR('',#10855,3.5);
#3136=VECTOR('',#10862,5.);
#3137=VECTOR('',#10873,3.);
#3138=VECTOR('',#10878,3.);
#3139=VECTOR('',#10881,3.);
#3140=VECTOR('',#10884,3.);
#3141=VECTOR('',#10887,3.);
#3142=VECTOR('',#10890,3.);
#3143=VECTOR('',#10893,3.);
#3144=VECTOR('',#10896,3.);
#3145=VECTOR('',#10899,3.);
#3146=VECTOR('',#10902,3.);
#3147=VECTOR('',#10905,3.);
#3148=VECTOR('',#10908,3.);
#3149=VECTOR('',#10911,3.);
#3150=VECTOR('',#10914,3.);
#3151=VECTOR('',#10917,3.);
#3152=VECTOR('',#10920,3.);
#3153=VECTOR('',#10923,3.);
#3154=VECTOR('',#10926,3.);
#3155=VECTOR('',#10929,3.);
#3156=VECTOR('',#10932,2.37175);
#3157=VECTOR('',#10937,2.37175);
#3158=VECTOR('',#10940,2.37175);
#3159=VECTOR('',#10943,2.37175);
#3160=VECTOR('',#10946,2.37175);
#3161=VECTOR('',#10949,2.37175);
#3162=VECTOR('',#10952,2.37175);
#3163=VECTOR('',#10955,2.37175);
#3164=VECTOR('',#10958,2.37175);
#3165=VECTOR('',#10961,2.37175);
#3166=VECTOR('',#10964,2.37175);
#3167=VECTOR('',#10967,2.37175);
#3168=VECTOR('',#10970,2.37175);
#3169=VECTOR('',#10973,2.37175);
#3170=VECTOR('',#10976,2.37175);
#3171=VECTOR('',#10979,2.37175);
#3172=VECTOR('',#10982,2.37175);
#3173=VECTOR('',#10985,2.37175);
#3174=VECTOR('',#10988,2.37175);
#3175=VECTOR('',#10993,2.5);
#3176=VECTOR('',#11004,10.);
#3177=VECTOR('',#11005,10.);
#3178=VECTOR('',#11006,10.);
#3179=VECTOR('',#11007,10.);
#3180=VECTOR('',#11010,10.);
#3181=VECTOR('',#11011,10.);
#3182=VECTOR('',#11012,10.);
#3183=VECTOR('',#11015,10.);
#3184=VECTOR('',#11016,10.);
#3185=VECTOR('',#11017,10.);
#3186=VECTOR('',#11020,10.);
#3187=VECTOR('',#11021,10.);
#3188=VECTOR('',#11022,10.);
#3189=VECTOR('',#11025,10.);
#3190=VECTOR('',#11026,10.);
#3191=VECTOR('',#11027,10.);
#3192=VECTOR('',#11030,10.);
#3193=VECTOR('',#11031,10.);
#3194=VECTOR('',#11040,5.);
#3195=VECTOR('',#11051,3.);
#3196=VECTOR('',#11056,3.);
#3197=VECTOR('',#11059,3.);
#3198=VECTOR('',#11062,3.);
#3199=VECTOR('',#11065,3.);
#3200=VECTOR('',#11068,3.);
#3201=VECTOR('',#11071,3.);
#3202=VECTOR('',#11074,3.);
#3203=VECTOR('',#11077,3.);
#3204=VECTOR('',#11080,3.);
#3205=VECTOR('',#11083,3.);
#3206=VECTOR('',#11086,2.37175);
#3207=VECTOR('',#11091,2.37175);
#3208=VECTOR('',#11094,2.37175);
#3209=VECTOR('',#11097,2.37175);
#3210=VECTOR('',#11100,2.37175);
#3211=VECTOR('',#11103,2.37175);
#3212=VECTOR('',#11106,2.37175);
#3213=VECTOR('',#11109,2.37175);
#3214=VECTOR('',#11112,2.37175);
#3215=VECTOR('',#11115,2.37175);
#3216=VECTOR('',#11118,2.37175);
#3217=VECTOR('',#11123,2.5);
#3218=VECTOR('',#11134,10.);
#3219=VECTOR('',#11135,10.);
#3220=VECTOR('',#11136,10.);
#3221=VECTOR('',#11137,10.);
#3222=VECTOR('',#11140,10.);
#3223=VECTOR('',#11141,10.);
#3224=VECTOR('',#11142,10.);
#3225=VECTOR('',#11145,10.);
#3226=VECTOR('',#11146,10.);
#3227=VECTOR('',#11147,10.);
#3228=VECTOR('',#11150,10.);
#3229=VECTOR('',#11151,10.);
#3230=VECTOR('',#11152,10.);
#3231=VECTOR('',#11155,10.);
#3232=VECTOR('',#11156,10.);
#3233=VECTOR('',#11157,10.);
#3234=VECTOR('',#11160,10.);
#3235=VECTOR('',#11161,10.);
#3236=VECTOR('',#11170,5.);
#3237=VECTOR('',#11183,3.5);
#3238=VECTOR('',#11190,7.);
#3239=VECTOR('',#11201,3.);
#3240=VECTOR('',#11206,3.);
#3241=VECTOR('',#11209,3.);
#3242=VECTOR('',#11212,3.);
#3243=VECTOR('',#11215,3.);
#3244=VECTOR('',#11220,3.0735);
#3245=VECTOR('',#11225,3.0735);
#3246=VECTOR('',#11228,3.0735);
#3247=VECTOR('',#11231,3.0735);
#3248=VECTOR('',#11234,3.0735);
#3249=VECTOR('',#11241,10.);
#3250=VECTOR('',#11242,10.);
#3251=VECTOR('',#11243,10.);
#3252=VECTOR('',#11244,10.);
#3253=VECTOR('',#11245,10.);
#3254=VECTOR('',#11246,10.);
#3255=VECTOR('',#11251,10.);
#3256=VECTOR('',#11252,10.);
#3257=VECTOR('',#11253,10.);
#3258=VECTOR('',#11256,10.);
#3259=VECTOR('',#11257,10.);
#3260=VECTOR('',#11260,10.);
#3261=VECTOR('',#11261,10.);
#3262=VECTOR('',#11264,10.);
#3263=VECTOR('',#11265,10.);
#3264=VECTOR('',#11268,10.);
#3265=VECTOR('',#11269,10.);
#3266=VECTOR('',#11272,10.);
#3267=VERTEX_POINT('',#11352);
#3268=VERTEX_POINT('',#11353);
#3269=VERTEX_POINT('',#11355);
#3270=VERTEX_POINT('',#11360);
#3271=VERTEX_POINT('',#11362);
#3272=VERTEX_POINT('',#11365);
#3273=VERTEX_POINT('',#11378);
#3274=VERTEX_POINT('',#11379);
#3275=VERTEX_POINT('',#11426);
#3276=VERTEX_POINT('',#11427);
#3277=VERTEX_POINT('',#11477);
#3278=VERTEX_POINT('',#11478);
#3279=VERTEX_POINT('',#11525);
#3280=VERTEX_POINT('',#11526);
#3281=VERTEX_POINT('',#11573);
#3282=VERTEX_POINT('',#11574);
#3283=VERTEX_POINT('',#11624);
#3284=VERTEX_POINT('',#11625);
#3285=VERTEX_POINT('',#11675);
#3286=VERTEX_POINT('',#11676);
#3287=VERTEX_POINT('',#11723);
#3288=VERTEX_POINT('',#11724);
#3289=VERTEX_POINT('',#11774);
#3290=VERTEX_POINT('',#11775);
#3291=VERTEX_POINT('',#11825);
#3292=VERTEX_POINT('',#11826);
#3293=VERTEX_POINT('',#11873);
#3294=VERTEX_POINT('',#11874);
#3295=VERTEX_POINT('',#11921);
#3296=VERTEX_POINT('',#11922);
#3297=VERTEX_POINT('',#11972);
#3298=VERTEX_POINT('',#11973);
#3299=VERTEX_POINT('',#12023);
#3300=VERTEX_POINT('',#12024);
#3301=VERTEX_POINT('',#12071);
#3302=VERTEX_POINT('',#12072);
#3303=VERTEX_POINT('',#12122);
#3304=VERTEX_POINT('',#12123);
#3305=VERTEX_POINT('',#12125);
#3306=VERTEX_POINT('',#12139);
#3307=VERTEX_POINT('',#12161);
#3308=VERTEX_POINT('',#12162);
#3309=VERTEX_POINT('',#12164);
#3310=VERTEX_POINT('',#12173);
#3311=VERTEX_POINT('',#12185);
#3312=VERTEX_POINT('',#12186);
#3313=VERTEX_POINT('',#12209);
#3314=VERTEX_POINT('',#12210);
#3315=VERTEX_POINT('',#12234);
#3316=VERTEX_POINT('',#12235);
#3317=VERTEX_POINT('',#12258);
#3318=VERTEX_POINT('',#12259);
#3319=VERTEX_POINT('',#12283);
#3320=VERTEX_POINT('',#12284);
#3321=VERTEX_POINT('',#12307);
#3322=VERTEX_POINT('',#12308);
#3323=VERTEX_POINT('',#12332);
#3324=VERTEX_POINT('',#12333);
#3325=VERTEX_POINT('',#12357);
#3326=VERTEX_POINT('',#12358);
#3327=VERTEX_POINT('',#12381);
#3328=VERTEX_POINT('',#12382);
#3329=VERTEX_POINT('',#12406);
#3330=VERTEX_POINT('',#12407);
#3331=VERTEX_POINT('',#12430);
#3332=VERTEX_POINT('',#12431);
#3333=VERTEX_POINT('',#12455);
#3334=VERTEX_POINT('',#12456);
#3335=VERTEX_POINT('',#12479);
#3336=VERTEX_POINT('',#12480);
#3337=VERTEX_POINT('',#12504);
#3338=VERTEX_POINT('',#12505);
#3339=VERTEX_POINT('',#12529);
#3340=VERTEX_POINT('',#12530);
#3341=VERTEX_POINT('',#12553);
#3342=VERTEX_POINT('',#12554);
#3343=VERTEX_POINT('',#12556);
#3344=VERTEX_POINT('',#12562);
#3345=VERTEX_POINT('',#12570);
#3346=VERTEX_POINT('',#12571);
#3347=VERTEX_POINT('',#12573);
#3348=VERTEX_POINT('',#12578);
#3349=VERTEX_POINT('',#12580);
#3350=VERTEX_POINT('',#12583);
#3351=VERTEX_POINT('',#12596);
#3352=VERTEX_POINT('',#12597);
#3353=VERTEX_POINT('',#12644);
#3354=VERTEX_POINT('',#12645);
#3355=VERTEX_POINT('',#12695);
#3356=VERTEX_POINT('',#12696);
#3357=VERTEX_POINT('',#12743);
#3358=VERTEX_POINT('',#12744);
#3359=VERTEX_POINT('',#12791);
#3360=VERTEX_POINT('',#12792);
#3361=VERTEX_POINT('',#12842);
#3362=VERTEX_POINT('',#12843);
#3363=VERTEX_POINT('',#12893);
#3364=VERTEX_POINT('',#12894);
#3365=VERTEX_POINT('',#12941);
#3366=VERTEX_POINT('',#12942);
#3367=VERTEX_POINT('',#12992);
#3368=VERTEX_POINT('',#12993);
#3369=VERTEX_POINT('',#13043);
#3370=VERTEX_POINT('',#13044);
#3371=VERTEX_POINT('',#13091);
#3372=VERTEX_POINT('',#13092);
#3373=VERTEX_POINT('',#13139);
#3374=VERTEX_POINT('',#13140);
#3375=VERTEX_POINT('',#13190);
#3376=VERTEX_POINT('',#13191);
#3377=VERTEX_POINT('',#13241);
#3378=VERTEX_POINT('',#13242);
#3379=VERTEX_POINT('',#13289);
#3380=VERTEX_POINT('',#13290);
#3381=VERTEX_POINT('',#13340);
#3382=VERTEX_POINT('',#13341);
#3383=VERTEX_POINT('',#13343);
#3384=VERTEX_POINT('',#13357);
#3385=VERTEX_POINT('',#13379);
#3386=VERTEX_POINT('',#13380);
#3387=VERTEX_POINT('',#13382);
#3388=VERTEX_POINT('',#13391);
#3389=VERTEX_POINT('',#13403);
#3390=VERTEX_POINT('',#13404);
#3391=VERTEX_POINT('',#13427);
#3392=VERTEX_POINT('',#13428);
#3393=VERTEX_POINT('',#13452);
#3394=VERTEX_POINT('',#13453);
#3395=VERTEX_POINT('',#13476);
#3396=VERTEX_POINT('',#13477);
#3397=VERTEX_POINT('',#13501);
#3398=VERTEX_POINT('',#13502);
#3399=VERTEX_POINT('',#13525);
#3400=VERTEX_POINT('',#13526);
#3401=VERTEX_POINT('',#13550);
#3402=VERTEX_POINT('',#13551);
#3403=VERTEX_POINT('',#13575);
#3404=VERTEX_POINT('',#13576);
#3405=VERTEX_POINT('',#13599);
#3406=VERTEX_POINT('',#13600);
#3407=VERTEX_POINT('',#13624);
#3408=VERTEX_POINT('',#13625);
#3409=VERTEX_POINT('',#13648);
#3410=VERTEX_POINT('',#13649);
#3411=VERTEX_POINT('',#13673);
#3412=VERTEX_POINT('',#13674);
#3413=VERTEX_POINT('',#13697);
#3414=VERTEX_POINT('',#13698);
#3415=VERTEX_POINT('',#13722);
#3416=VERTEX_POINT('',#13723);
#3417=VERTEX_POINT('',#13747);
#3418=VERTEX_POINT('',#13748);
#3419=VERTEX_POINT('',#13771);
#3420=VERTEX_POINT('',#13772);
#3421=VERTEX_POINT('',#13774);
#3422=VERTEX_POINT('',#13780);
#3423=VERTEX_POINT('',#13788);
#3424=VERTEX_POINT('',#13789);
#3425=VERTEX_POINT('',#13791);
#3426=VERTEX_POINT('',#13796);
#3427=VERTEX_POINT('',#13798);
#3428=VERTEX_POINT('',#13801);
#3429=VERTEX_POINT('',#13814);
#3430=VERTEX_POINT('',#13815);
#3431=VERTEX_POINT('',#13862);
#3432=VERTEX_POINT('',#13863);
#3433=VERTEX_POINT('',#13913);
#3434=VERTEX_POINT('',#13914);
#3435=VERTEX_POINT('',#13961);
#3436=VERTEX_POINT('',#13962);
#3437=VERTEX_POINT('',#14009);
#3438=VERTEX_POINT('',#14010);
#3439=VERTEX_POINT('',#14060);
#3440=VERTEX_POINT('',#14061);
#3441=VERTEX_POINT('',#14111);
#3442=VERTEX_POINT('',#14112);
#3443=VERTEX_POINT('',#14159);
#3444=VERTEX_POINT('',#14160);
#3445=VERTEX_POINT('',#14210);
#3446=VERTEX_POINT('',#14211);
#3447=VERTEX_POINT('',#14261);
#3448=VERTEX_POINT('',#14262);
#3449=VERTEX_POINT('',#14309);
#3450=VERTEX_POINT('',#14310);
#3451=VERTEX_POINT('',#14357);
#3452=VERTEX_POINT('',#14358);
#3453=VERTEX_POINT('',#14408);
#3454=VERTEX_POINT('',#14409);
#3455=VERTEX_POINT('',#14459);
#3456=VERTEX_POINT('',#14460);
#3457=VERTEX_POINT('',#14507);
#3458=VERTEX_POINT('',#14508);
#3459=VERTEX_POINT('',#14558);
#3460=VERTEX_POINT('',#14559);
#3461=VERTEX_POINT('',#14561);
#3462=VERTEX_POINT('',#14575);
#3463=VERTEX_POINT('',#14597);
#3464=VERTEX_POINT('',#14598);
#3465=VERTEX_POINT('',#14600);
#3466=VERTEX_POINT('',#14609);
#3467=VERTEX_POINT('',#14621);
#3468=VERTEX_POINT('',#14622);
#3469=VERTEX_POINT('',#14645);
#3470=VERTEX_POINT('',#14646);
#3471=VERTEX_POINT('',#14670);
#3472=VERTEX_POINT('',#14671);
#3473=VERTEX_POINT('',#14694);
#3474=VERTEX_POINT('',#14695);
#3475=VERTEX_POINT('',#14719);
#3476=VERTEX_POINT('',#14720);
#3477=VERTEX_POINT('',#14743);
#3478=VERTEX_POINT('',#14744);
#3479=VERTEX_POINT('',#14768);
#3480=VERTEX_POINT('',#14769);
#3481=VERTEX_POINT('',#14793);
#3482=VERTEX_POINT('',#14794);
#3483=VERTEX_POINT('',#14817);
#3484=VERTEX_POINT('',#14818);
#3485=VERTEX_POINT('',#14842);
#3486=VERTEX_POINT('',#14843);
#3487=VERTEX_POINT('',#14866);
#3488=VERTEX_POINT('',#14867);
#3489=VERTEX_POINT('',#14891);
#3490=VERTEX_POINT('',#14892);
#3491=VERTEX_POINT('',#14915);
#3492=VERTEX_POINT('',#14916);
#3493=VERTEX_POINT('',#14940);
#3494=VERTEX_POINT('',#14941);
#3495=VERTEX_POINT('',#14965);
#3496=VERTEX_POINT('',#14966);
#3497=VERTEX_POINT('',#14989);
#3498=VERTEX_POINT('',#14990);
#3499=VERTEX_POINT('',#14992);
#3500=VERTEX_POINT('',#14998);
#3501=VERTEX_POINT('',#15006);
#3502=VERTEX_POINT('',#15007);
#3503=VERTEX_POINT('',#15009);
#3504=VERTEX_POINT('',#15014);
#3505=VERTEX_POINT('',#15016);
#3506=VERTEX_POINT('',#15019);
#3507=VERTEX_POINT('',#15032);
#3508=VERTEX_POINT('',#15033);
#3509=VERTEX_POINT('',#15080);
#3510=VERTEX_POINT('',#15081);
#3511=VERTEX_POINT('',#15131);
#3512=VERTEX_POINT('',#15132);
#3513=VERTEX_POINT('',#15179);
#3514=VERTEX_POINT('',#15180);
#3515=VERTEX_POINT('',#15227);
#3516=VERTEX_POINT('',#15228);
#3517=VERTEX_POINT('',#15278);
#3518=VERTEX_POINT('',#15279);
#3519=VERTEX_POINT('',#15329);
#3520=VERTEX_POINT('',#15330);
#3521=VERTEX_POINT('',#15377);
#3522=VERTEX_POINT('',#15378);
#3523=VERTEX_POINT('',#15428);
#3524=VERTEX_POINT('',#15429);
#3525=VERTEX_POINT('',#15479);
#3526=VERTEX_POINT('',#15480);
#3527=VERTEX_POINT('',#15527);
#3528=VERTEX_POINT('',#15528);
#3529=VERTEX_POINT('',#15575);
#3530=VERTEX_POINT('',#15576);
#3531=VERTEX_POINT('',#15626);
#3532=VERTEX_POINT('',#15627);
#3533=VERTEX_POINT('',#15677);
#3534=VERTEX_POINT('',#15678);
#3535=VERTEX_POINT('',#15725);
#3536=VERTEX_POINT('',#15726);
#3537=VERTEX_POINT('',#15776);
#3538=VERTEX_POINT('',#15777);
#3539=VERTEX_POINT('',#15779);
#3540=VERTEX_POINT('',#15793);
#3541=VERTEX_POINT('',#15815);
#3542=VERTEX_POINT('',#15816);
#3543=VERTEX_POINT('',#15818);
#3544=VERTEX_POINT('',#15827);
#3545=VERTEX_POINT('',#15839);
#3546=VERTEX_POINT('',#15840);
#3547=VERTEX_POINT('',#15863);
#3548=VERTEX_POINT('',#15864);
#3549=VERTEX_POINT('',#15888);
#3550=VERTEX_POINT('',#15889);
#3551=VERTEX_POINT('',#15912);
#3552=VERTEX_POINT('',#15913);
#3553=VERTEX_POINT('',#15937);
#3554=VERTEX_POINT('',#15938);
#3555=VERTEX_POINT('',#15961);
#3556=VERTEX_POINT('',#15962);
#3557=VERTEX_POINT('',#15986);
#3558=VERTEX_POINT('',#15987);
#3559=VERTEX_POINT('',#16011);
#3560=VERTEX_POINT('',#16012);
#3561=VERTEX_POINT('',#16035);
#3562=VERTEX_POINT('',#16036);
#3563=VERTEX_POINT('',#16060);
#3564=VERTEX_POINT('',#16061);
#3565=VERTEX_POINT('',#16084);
#3566=VERTEX_POINT('',#16085);
#3567=VERTEX_POINT('',#16109);
#3568=VERTEX_POINT('',#16110);
#3569=VERTEX_POINT('',#16133);
#3570=VERTEX_POINT('',#16134);
#3571=VERTEX_POINT('',#16158);
#3572=VERTEX_POINT('',#16159);
#3573=VERTEX_POINT('',#16183);
#3574=VERTEX_POINT('',#16184);
#3575=VERTEX_POINT('',#16207);
#3576=VERTEX_POINT('',#16208);
#3577=VERTEX_POINT('',#16210);
#3578=VERTEX_POINT('',#16216);
#3579=VERTEX_POINT('',#21588);
#3580=VERTEX_POINT('',#21589);
#3581=VERTEX_POINT('',#21591);
#3582=VERTEX_POINT('',#21593);
#3583=VERTEX_POINT('',#21597);
#3584=VERTEX_POINT('',#21599);
#3585=VERTEX_POINT('',#21603);
#3586=VERTEX_POINT('',#21605);
#3587=VERTEX_POINT('',#21612);
#3588=VERTEX_POINT('',#21613);
#3589=VERTEX_POINT('',#21615);
#3590=VERTEX_POINT('',#21617);
#3591=VERTEX_POINT('',#21621);
#3592=VERTEX_POINT('',#21623);
#3593=VERTEX_POINT('',#21627);
#3594=VERTEX_POINT('',#21629);
#3595=VERTEX_POINT('',#21639);
#3596=VERTEX_POINT('',#21641);
#3597=VERTEX_POINT('',#21645);
#3598=VERTEX_POINT('',#21647);
#3599=VERTEX_POINT('',#21651);
#3600=VERTEX_POINT('',#21653);
#3601=VERTEX_POINT('',#21657);
#3602=VERTEX_POINT('',#21659);
#3603=VERTEX_POINT('',#21663);
#3604=VERTEX_POINT('',#21665);
#3605=VERTEX_POINT('',#21669);
#3606=VERTEX_POINT('',#21670);
#3607=VERTEX_POINT('',#21672);
#3608=VERTEX_POINT('',#21674);
#3609=VERTEX_POINT('',#21678);
#3610=VERTEX_POINT('',#21680);
#3611=VERTEX_POINT('',#21684);
#3612=VERTEX_POINT('',#21686);
#3613=VERTEX_POINT('',#21696);
#3614=VERTEX_POINT('',#21697);
#3615=VERTEX_POINT('',#21699);
#3616=VERTEX_POINT('',#21701);
#3617=VERTEX_POINT('',#21705);
#3618=VERTEX_POINT('',#21707);
#3619=VERTEX_POINT('',#21711);
#3620=VERTEX_POINT('',#21713);
#3621=VERTEX_POINT('',#21720);
#3622=VERTEX_POINT('',#21721);
#3623=VERTEX_POINT('',#21723);
#3624=VERTEX_POINT('',#21725);
#3625=VERTEX_POINT('',#21729);
#3626=VERTEX_POINT('',#21731);
#3627=VERTEX_POINT('',#21735);
#3628=VERTEX_POINT('',#21737);
#3629=VERTEX_POINT('',#21747);
#3630=VERTEX_POINT('',#21748);
#3631=VERTEX_POINT('',#21750);
#3632=VERTEX_POINT('',#21770);
#3633=VERTEX_POINT('',#21772);
#3634=VERTEX_POINT('',#21777);
#3635=VERTEX_POINT('',#21803);
#3636=VERTEX_POINT('',#21804);
#3637=VERTEX_POINT('',#21854);
#3638=VERTEX_POINT('',#21855);
#3639=VERTEX_POINT('',#21902);
#3640=VERTEX_POINT('',#21903);
#3641=VERTEX_POINT('',#21953);
#3642=VERTEX_POINT('',#21954);
#3643=VERTEX_POINT('',#22004);
#3644=VERTEX_POINT('',#22005);
#3645=VERTEX_POINT('',#22052);
#3646=VERTEX_POINT('',#22053);
#3647=VERTEX_POINT('',#22100);
#3648=VERTEX_POINT('',#22101);
#3649=VERTEX_POINT('',#22151);
#3650=VERTEX_POINT('',#22152);
#3651=VERTEX_POINT('',#22199);
#3652=VERTEX_POINT('',#22200);
#3653=VERTEX_POINT('',#22247);
#3654=VERTEX_POINT('',#22248);
#3655=VERTEX_POINT('',#22298);
#3656=VERTEX_POINT('',#22299);
#3657=VERTEX_POINT('',#22349);
#3658=VERTEX_POINT('',#22350);
#3659=VERTEX_POINT('',#22397);
#3660=VERTEX_POINT('',#22398);
#3661=VERTEX_POINT('',#22448);
#3662=VERTEX_POINT('',#22449);
#3663=VERTEX_POINT('',#22451);
#3664=VERTEX_POINT('',#22465);
#3665=VERTEX_POINT('',#22487);
#3666=VERTEX_POINT('',#22488);
#3667=VERTEX_POINT('',#22490);
#3668=VERTEX_POINT('',#22497);
#3669=VERTEX_POINT('',#22507);
#3670=VERTEX_POINT('',#22508);
#3671=VERTEX_POINT('',#22531);
#3672=VERTEX_POINT('',#22532);
#3673=VERTEX_POINT('',#22556);
#3674=VERTEX_POINT('',#22557);
#3675=VERTEX_POINT('',#22581);
#3676=VERTEX_POINT('',#22582);
#3677=VERTEX_POINT('',#22605);
#3678=VERTEX_POINT('',#22606);
#3679=VERTEX_POINT('',#22630);
#3680=VERTEX_POINT('',#22631);
#3681=VERTEX_POINT('',#22654);
#3682=VERTEX_POINT('',#22655);
#3683=VERTEX_POINT('',#22679);
#3684=VERTEX_POINT('',#22680);
#3685=VERTEX_POINT('',#22704);
#3686=VERTEX_POINT('',#22705);
#3687=VERTEX_POINT('',#22728);
#3688=VERTEX_POINT('',#22729);
#3689=VERTEX_POINT('',#22753);
#3690=VERTEX_POINT('',#22754);
#3691=VERTEX_POINT('',#22777);
#3692=VERTEX_POINT('',#22778);
#3693=VERTEX_POINT('',#22802);
#3694=VERTEX_POINT('',#22803);
#3695=VERTEX_POINT('',#22827);
#3696=VERTEX_POINT('',#22828);
#3697=VERTEX_POINT('',#22851);
#3698=VERTEX_POINT('',#22852);
#3699=VERTEX_POINT('',#22854);
#3700=VERTEX_POINT('',#22860);
#3701=VERTEX_POINT('',#24112);
#3702=VERTEX_POINT('',#24113);
#3703=VERTEX_POINT('',#24115);
#3704=VERTEX_POINT('',#24117);
#3705=VERTEX_POINT('',#24121);
#3706=VERTEX_POINT('',#24123);
#3707=VERTEX_POINT('',#24127);
#3708=VERTEX_POINT('',#24129);
#3709=VERTEX_POINT('',#24137);
#3710=VERTEX_POINT('',#24139);
#3711=VERTEX_POINT('',#24143);
#3712=VERTEX_POINT('',#24146);
#3713=VERTEX_POINT('',#24149);
#3714=VERTEX_POINT('',#24153);
#3715=VERTEX_POINT('',#24154);
#3716=VERTEX_POINT('',#24156);
#3717=VERTEX_POINT('',#24158);
#3718=VERTEX_POINT('',#24162);
#3719=VERTEX_POINT('',#24164);
#3720=VERTEX_POINT('',#24168);
#3721=VERTEX_POINT('',#24170);
#3722=VERTEX_POINT('',#24174);
#3723=VERTEX_POINT('',#24176);
#3724=VERTEX_POINT('',#24180);
#3725=VERTEX_POINT('',#24182);
#3726=VERTEX_POINT('',#24190);
#3727=VERTEX_POINT('',#24192);
#3728=VERTEX_POINT('',#24195);
#3729=VERTEX_POINT('',#24204);
#3730=VERTEX_POINT('',#24205);
#3731=VERTEX_POINT('',#24207);
#3732=VERTEX_POINT('',#24209);
#3733=VERTEX_POINT('',#24213);
#3734=VERTEX_POINT('',#24215);
#3735=VERTEX_POINT('',#24219);
#3736=VERTEX_POINT('',#24221);
#3737=VERTEX_POINT('',#24225);
#3738=VERTEX_POINT('',#24227);
#3739=VERTEX_POINT('',#24231);
#3740=VERTEX_POINT('',#24233);
#3741=VERTEX_POINT('',#24240);
#3742=VERTEX_POINT('',#24241);
#3743=VERTEX_POINT('',#24243);
#3744=VERTEX_POINT('',#24245);
#3745=VERTEX_POINT('',#24249);
#3746=VERTEX_POINT('',#24251);
#3747=VERTEX_POINT('',#24255);
#3748=VERTEX_POINT('',#24257);
#3749=VERTEX_POINT('',#24267);
#3750=VERTEX_POINT('',#24269);
#3751=VERTEX_POINT('',#24273);
#3752=VERTEX_POINT('',#24275);
#3753=VERTEX_POINT('',#24282);
#3754=VERTEX_POINT('',#24283);
#3755=VERTEX_POINT('',#24285);
#3756=VERTEX_POINT('',#24287);
#3757=VERTEX_POINT('',#24291);
#3758=VERTEX_POINT('',#24292);
#3759=VERTEX_POINT('',#24294);
#3760=VERTEX_POINT('',#24296);
#3761=VERTEX_POINT('',#24309);
#3762=VERTEX_POINT('',#24311);
#3763=VERTEX_POINT('',#24315);
#3764=VERTEX_POINT('',#24317);
#3765=VERTEX_POINT('',#24324);
#3766=VERTEX_POINT('',#24325);
#3767=VERTEX_POINT('',#24327);
#3768=VERTEX_POINT('',#24338);
#3769=VERTEX_POINT('',#24348);
#3770=VERTEX_POINT('',#24349);
#3771=VERTEX_POINT('',#24396);
#3772=VERTEX_POINT('',#24397);
#3773=VERTEX_POINT('',#24444);
#3774=VERTEX_POINT('',#24445);
#3775=VERTEX_POINT('',#24495);
#3776=VERTEX_POINT('',#24496);
#3777=VERTEX_POINT('',#24546);
#3778=VERTEX_POINT('',#24547);
#3779=VERTEX_POINT('',#24594);
#3780=VERTEX_POINT('',#24595);
#3781=VERTEX_POINT('',#24642);
#3782=VERTEX_POINT('',#24643);
#3783=VERTEX_POINT('',#24696);
#3784=VERTEX_POINT('',#24697);
#3785=VERTEX_POINT('',#24744);
#3786=VERTEX_POINT('',#24745);
#3787=VERTEX_POINT('',#24792);
#3788=VERTEX_POINT('',#24793);
#3789=VERTEX_POINT('',#24795);
#3790=VERTEX_POINT('',#24806);
#3791=VERTEX_POINT('',#24817);
#3792=VERTEX_POINT('',#24818);
#3793=VERTEX_POINT('',#24842);
#3794=VERTEX_POINT('',#24843);
#3795=VERTEX_POINT('',#24866);
#3796=VERTEX_POINT('',#24867);
#3797=VERTEX_POINT('',#24891);
#3798=VERTEX_POINT('',#24892);
#3799=VERTEX_POINT('',#24916);
#3800=VERTEX_POINT('',#24917);
#3801=VERTEX_POINT('',#24940);
#3802=VERTEX_POINT('',#24941);
#3803=VERTEX_POINT('',#24964);
#3804=VERTEX_POINT('',#24965);
#3805=VERTEX_POINT('',#24990);
#3806=VERTEX_POINT('',#24991);
#3807=VERTEX_POINT('',#25014);
#3808=VERTEX_POINT('',#25015);
#3809=VERTEX_POINT('',#25038);
#3810=VERTEX_POINT('',#25244);
#3811=VERTEX_POINT('',#25303);
#3812=VERTEX_POINT('',#25333);
#3813=VERTEX_POINT('',#25616);
#3814=VERTEX_POINT('',#25730);
#3815=VERTEX_POINT('',#26135);
#3816=VERTEX_POINT('',#26136);
#3817=VERTEX_POINT('',#26138);
#3818=VERTEX_POINT('',#26140);
#3819=VERTEX_POINT('',#26144);
#3820=VERTEX_POINT('',#26146);
#3821=VERTEX_POINT('',#26150);
#3822=VERTEX_POINT('',#26152);
#3823=VERTEX_POINT('',#26156);
#3824=VERTEX_POINT('',#26158);
#3825=VERTEX_POINT('',#26162);
#3826=VERTEX_POINT('',#26164);
#3827=VERTEX_POINT('',#26172);
#3828=VERTEX_POINT('',#26175);
#3829=VERTEX_POINT('',#26182);
#3830=VERTEX_POINT('',#26183);
#3831=VERTEX_POINT('',#26185);
#3832=VERTEX_POINT('',#26187);
#3833=VERTEX_POINT('',#26191);
#3834=VERTEX_POINT('',#26193);
#3835=VERTEX_POINT('',#26195);
#3836=VERTEX_POINT('',#26197);
#3837=VERTEX_POINT('',#26199);
#3838=VERTEX_POINT('',#26201);
#3839=VERTEX_POINT('',#26204);
#3840=VERTEX_POINT('',#26206);
#3841=VERTEX_POINT('',#26209);
#3842=VERTEX_POINT('',#26213);
#3843=VERTEX_POINT('',#26217);
#3844=VERTEX_POINT('',#26218);
#3845=VERTEX_POINT('',#26223);
#3846=VERTEX_POINT('',#26225);
#3847=VERTEX_POINT('',#26231);
#3848=VERTEX_POINT('',#26234);
#3849=VERTEX_POINT('',#26237);
#3850=VERTEX_POINT('',#26241);
#3851=VERTEX_POINT('',#26245);
#3852=VERTEX_POINT('',#26249);
#3853=VERTEX_POINT('',#26257);
#3854=VERTEX_POINT('',#26259);
#3855=VERTEX_POINT('',#26263);
#3856=VERTEX_POINT('',#26266);
#3857=VERTEX_POINT('',#26269);
#3858=VERTEX_POINT('',#26273);
#3859=VERTEX_POINT('',#26275);
#3860=VERTEX_POINT('',#26278);
#3861=VERTEX_POINT('',#26287);
#3862=VERTEX_POINT('',#26288);
#3863=VERTEX_POINT('',#26290);
#3864=VERTEX_POINT('',#26292);
#3865=VERTEX_POINT('',#26296);
#3866=VERTEX_POINT('',#26297);
#3867=VERTEX_POINT('',#26299);
#3868=VERTEX_POINT('',#26301);
#3869=VERTEX_POINT('',#26314);
#3870=VERTEX_POINT('',#26315);
#3871=VERTEX_POINT('',#26317);
#3872=VERTEX_POINT('',#26319);
#3873=VERTEX_POINT('',#26323);
#3874=VERTEX_POINT('',#26324);
#3875=VERTEX_POINT('',#26326);
#3876=VERTEX_POINT('',#26328);
#3877=VERTEX_POINT('',#26332);
#3878=VERTEX_POINT('',#26334);
#3879=VERTEX_POINT('',#26337);
#3880=VERTEX_POINT('',#26339);
#3881=VERTEX_POINT('',#26342);
#3882=VERTEX_POINT('',#26344);
#3883=VERTEX_POINT('',#26347);
#3884=VERTEX_POINT('',#26351);
#3885=VERTEX_POINT('',#26355);
#3886=VERTEX_POINT('',#26359);
#3887=VERTEX_POINT('',#26362);
#3888=VERTEX_POINT('',#26365);
#3889=VERTEX_POINT('',#26369);
#3890=VERTEX_POINT('',#26375);
#3891=VERTEX_POINT('',#26383);
#3892=VERTEX_POINT('',#26385);
#3893=VERTEX_POINT('',#26389);
#3894=VERTEX_POINT('',#26391);
#3895=VERTEX_POINT('',#26398);
#3896=VERTEX_POINT('',#26399);
#3897=VERTEX_POINT('',#26401);
#3898=VERTEX_POINT('',#26412);
#3899=VERTEX_POINT('',#26422);
#3900=VERTEX_POINT('',#26423);
#3901=VERTEX_POINT('',#26470);
#3902=VERTEX_POINT('',#26471);
#3903=VERTEX_POINT('',#26518);
#3904=VERTEX_POINT('',#26519);
#3905=VERTEX_POINT('',#26572);
#3906=VERTEX_POINT('',#26573);
#3907=VERTEX_POINT('',#26620);
#3908=VERTEX_POINT('',#26621);
#3909=VERTEX_POINT('',#26668);
#3910=VERTEX_POINT('',#26669);
#3911=VERTEX_POINT('',#26722);
#3912=VERTEX_POINT('',#26723);
#3913=VERTEX_POINT('',#26770);
#3914=VERTEX_POINT('',#26771);
#3915=VERTEX_POINT('',#26818);
#3916=VERTEX_POINT('',#26819);
#3917=VERTEX_POINT('',#26866);
#3918=VERTEX_POINT('',#26867);
#3919=VERTEX_POINT('',#26920);
#3920=VERTEX_POINT('',#26921);
#3921=VERTEX_POINT('',#26968);
#3922=VERTEX_POINT('',#26969);
#3923=VERTEX_POINT('',#27016);
#3924=VERTEX_POINT('',#27017);
#3925=VERTEX_POINT('',#27070);
#3926=VERTEX_POINT('',#27071);
#3927=VERTEX_POINT('',#27118);
#3928=VERTEX_POINT('',#27119);
#3929=VERTEX_POINT('',#27166);
#3930=VERTEX_POINT('',#27167);
#3931=VERTEX_POINT('',#27220);
#3932=VERTEX_POINT('',#27221);
#3933=VERTEX_POINT('',#27268);
#3934=VERTEX_POINT('',#27269);
#3935=VERTEX_POINT('',#27316);
#3936=VERTEX_POINT('',#27317);
#3937=VERTEX_POINT('',#27319);
#3938=VERTEX_POINT('',#27330);
#3939=VERTEX_POINT('',#27341);
#3940=VERTEX_POINT('',#27342);
#3941=VERTEX_POINT('',#27366);
#3942=VERTEX_POINT('',#27367);
#3943=VERTEX_POINT('',#27390);
#3944=VERTEX_POINT('',#27391);
#3945=VERTEX_POINT('',#27415);
#3946=VERTEX_POINT('',#27416);
#3947=VERTEX_POINT('',#27440);
#3948=VERTEX_POINT('',#27441);
#3949=VERTEX_POINT('',#27464);
#3950=VERTEX_POINT('',#27465);
#3951=VERTEX_POINT('',#27489);
#3952=VERTEX_POINT('',#27490);
#3953=VERTEX_POINT('',#27514);
#3954=VERTEX_POINT('',#27515);
#3955=VERTEX_POINT('',#27538);
#3956=VERTEX_POINT('',#27539);
#3957=VERTEX_POINT('',#27563);
#3958=VERTEX_POINT('',#27564);
#3959=VERTEX_POINT('',#27588);
#3960=VERTEX_POINT('',#27589);
#3961=VERTEX_POINT('',#27612);
#3962=VERTEX_POINT('',#27613);
#3963=VERTEX_POINT('',#27636);
#3964=VERTEX_POINT('',#27637);
#3965=VERTEX_POINT('',#27661);
#3966=VERTEX_POINT('',#27662);
#3967=VERTEX_POINT('',#27686);
#3968=VERTEX_POINT('',#27687);
#3969=VERTEX_POINT('',#27710);
#3970=VERTEX_POINT('',#27711);
#3971=VERTEX_POINT('',#27735);
#3972=VERTEX_POINT('',#27736);
#3973=VERTEX_POINT('',#27760);
#3974=VERTEX_POINT('',#27761);
#3975=VERTEX_POINT('',#27784);
#3976=VERTEX_POINT('',#28002);
#3977=VERTEX_POINT('',#28067);
#3978=VERTEX_POINT('',#28100);
#3979=VERTEX_POINT('',#28611);
#3980=VERTEX_POINT('',#28731);
#3981=VERTEX_POINT('',#29373);
#3982=VERTEX_POINT('',#29374);
#3983=VERTEX_POINT('',#29376);
#3984=VERTEX_POINT('',#29378);
#3985=VERTEX_POINT('',#29382);
#3986=VERTEX_POINT('',#29384);
#3987=VERTEX_POINT('',#29388);
#3988=VERTEX_POINT('',#29390);
#3989=VERTEX_POINT('',#29394);
#3990=VERTEX_POINT('',#29396);
#3991=VERTEX_POINT('',#29400);
#3992=VERTEX_POINT('',#29402);
#3993=VERTEX_POINT('',#29410);
#3994=VERTEX_POINT('',#29413);
#3995=VERTEX_POINT('',#29420);
#3996=VERTEX_POINT('',#29421);
#3997=VERTEX_POINT('',#29423);
#3998=VERTEX_POINT('',#29434);
#3999=VERTEX_POINT('',#29444);
#4000=VERTEX_POINT('',#29445);
#4001=VERTEX_POINT('',#29492);
#4002=VERTEX_POINT('',#29493);
#4003=VERTEX_POINT('',#29540);
#4004=VERTEX_POINT('',#29541);
#4005=VERTEX_POINT('',#29594);
#4006=VERTEX_POINT('',#29595);
#4007=VERTEX_POINT('',#29642);
#4008=VERTEX_POINT('',#29643);
#4009=VERTEX_POINT('',#29690);
#4010=VERTEX_POINT('',#29691);
#4011=VERTEX_POINT('',#29744);
#4012=VERTEX_POINT('',#29745);
#4013=VERTEX_POINT('',#29792);
#4014=VERTEX_POINT('',#29793);
#4015=VERTEX_POINT('',#29843);
#4016=VERTEX_POINT('',#29844);
#4017=VERTEX_POINT('',#29894);
#4018=VERTEX_POINT('',#29895);
#4019=VERTEX_POINT('',#29942);
#4020=VERTEX_POINT('',#29943);
#4021=VERTEX_POINT('',#29945);
#4022=VERTEX_POINT('',#29956);
#4023=VERTEX_POINT('',#29967);
#4024=VERTEX_POINT('',#29968);
#4025=VERTEX_POINT('',#29992);
#4026=VERTEX_POINT('',#29993);
#4027=VERTEX_POINT('',#30016);
#4028=VERTEX_POINT('',#30017);
#4029=VERTEX_POINT('',#30042);
#4030=VERTEX_POINT('',#30043);
#4031=VERTEX_POINT('',#30066);
#4032=VERTEX_POINT('',#30067);
#4033=VERTEX_POINT('',#30091);
#4034=VERTEX_POINT('',#30092);
#4035=VERTEX_POINT('',#30116);
#4036=VERTEX_POINT('',#30117);
#4037=VERTEX_POINT('',#30140);
#4038=VERTEX_POINT('',#30141);
#4039=VERTEX_POINT('',#30165);
#4040=VERTEX_POINT('',#30166);
#4041=VERTEX_POINT('',#30190);
#4042=VERTEX_POINT('',#30191);
#4043=VERTEX_POINT('',#30214);
#4044=VERTEX_POINT('',#30432);
#4045=VERTEX_POINT('',#30494);
#4046=VERTEX_POINT('',#30527);
#4047=VERTEX_POINT('',#30838);
#4048=VERTEX_POINT('',#30955);
#4049=VERTEX_POINT('',#31394);
#4050=VERTEX_POINT('',#31395);
#4051=VERTEX_POINT('',#31397);
#4052=VERTEX_POINT('',#31399);
#4053=VERTEX_POINT('',#31403);
#4054=VERTEX_POINT('',#31405);
#4055=VERTEX_POINT('',#31409);
#4056=VERTEX_POINT('',#31411);
#4057=VERTEX_POINT('',#31415);
#4058=VERTEX_POINT('',#31417);
#4059=VERTEX_POINT('',#31421);
#4060=VERTEX_POINT('',#31423);
#4061=VERTEX_POINT('',#31431);
#4062=VERTEX_POINT('',#31434);
#4063=VERTEX_POINT('',#31441);
#4064=VERTEX_POINT('',#31443);
#4065=VERTEX_POINT('',#31447);
#4066=VERTEX_POINT('',#31449);
#4067=VERTEX_POINT('',#31456);
#4068=VERTEX_POINT('',#31457);
#4069=VERTEX_POINT('',#31459);
#4070=VERTEX_POINT('',#31464);
#4071=VERTEX_POINT('',#31477);
#4072=VERTEX_POINT('',#31478);
#4073=VERTEX_POINT('',#31528);
#4074=VERTEX_POINT('',#31529);
#4075=VERTEX_POINT('',#31579);
#4076=VERTEX_POINT('',#31580);
#4077=VERTEX_POINT('',#31627);
#4078=VERTEX_POINT('',#31628);
#4079=VERTEX_POINT('',#31630);
#4080=VERTEX_POINT('',#31644);
#4081=VERTEX_POINT('',#31666);
#4082=VERTEX_POINT('',#31667);
#4083=VERTEX_POINT('',#31669);
#4084=VERTEX_POINT('',#31678);
#4085=VERTEX_POINT('',#31690);
#4086=VERTEX_POINT('',#31691);
#4087=VERTEX_POINT('',#31714);
#4088=VERTEX_POINT('',#31715);
#4089=VERTEX_POINT('',#31739);
#4090=VERTEX_POINT('',#31740);
#4091=VERTEX_POINT('',#31764);
#4092=VERTEX_POINT('',#31765);
#4093=VERTEX_POINT('',#31767);
#4094=VERTEX_POINT('',#31773);
#4095=VERTEX_POINT('',#32513);
#4096=VERTEX_POINT('',#32514);
#4097=VERTEX_POINT('',#32516);
#4098=VERTEX_POINT('',#32518);
#4099=VERTEX_POINT('',#32520);
#4100=VERTEX_POINT('',#32522);
#4101=VERTEX_POINT('',#32527);
#4102=VERTEX_POINT('',#32528);
#4103=VERTEX_POINT('',#32533);
#4104=VERTEX_POINT('',#32537);
#4105=VERTEX_POINT('',#32541);
#4106=VERTEX_POINT('',#32545);
#4107=EDGE_CURVE('',#3267,#3268,#2175,.T.);
#4108=EDGE_CURVE('',#3268,#3269,#1585,.T.);
#4109=EDGE_CURVE('',#3269,#3270,#1461,.T.);
#4110=EDGE_CURVE('',#3270,#3271,#2176,.T.);
#4111=EDGE_CURVE('',#3271,#3271,#1462,.F.);
#4112=EDGE_CURVE('',#3270,#3272,#1463,.T.);
#4113=EDGE_CURVE('',#3272,#3267,#1586,.T.);
#4114=EDGE_CURVE('',#3273,#3274,#2177,.T.);
#4115=EDGE_CURVE('',#3274,#3268,#1587,.T.);
#4116=EDGE_CURVE('',#3267,#3273,#1588,.T.);
#4117=EDGE_CURVE('',#3275,#3276,#2178,.T.);
#4118=EDGE_CURVE('',#3276,#3274,#1589,.T.);
#4119=EDGE_CURVE('',#3273,#3275,#1590,.T.);
#4120=EDGE_CURVE('',#3277,#3278,#2179,.T.);
#4121=EDGE_CURVE('',#3278,#3276,#1591,.T.);
#4122=EDGE_CURVE('',#3275,#3277,#1592,.T.);
#4123=EDGE_CURVE('',#3279,#3280,#2180,.T.);
#4124=EDGE_CURVE('',#3280,#3278,#1593,.T.);
#4125=EDGE_CURVE('',#3277,#3279,#1594,.T.);
#4126=EDGE_CURVE('',#3281,#3282,#2181,.T.);
#4127=EDGE_CURVE('',#3282,#3280,#1595,.T.);
#4128=EDGE_CURVE('',#3279,#3281,#1596,.T.);
#4129=EDGE_CURVE('',#3283,#3284,#2182,.T.);
#4130=EDGE_CURVE('',#3284,#3282,#1597,.T.);
#4131=EDGE_CURVE('',#3281,#3283,#1598,.T.);
#4132=EDGE_CURVE('',#3285,#3286,#2183,.T.);
#4133=EDGE_CURVE('',#3286,#3284,#1599,.T.);
#4134=EDGE_CURVE('',#3283,#3285,#1600,.T.);
#4135=EDGE_CURVE('',#3287,#3288,#2184,.T.);
#4136=EDGE_CURVE('',#3288,#3286,#1601,.T.);
#4137=EDGE_CURVE('',#3285,#3287,#1602,.T.);
#4138=EDGE_CURVE('',#3289,#3290,#2185,.T.);
#4139=EDGE_CURVE('',#3290,#3288,#1603,.T.);
#4140=EDGE_CURVE('',#3287,#3289,#1604,.T.);
#4141=EDGE_CURVE('',#3291,#3292,#2186,.T.);
#4142=EDGE_CURVE('',#3292,#3290,#1605,.T.);
#4143=EDGE_CURVE('',#3289,#3291,#1606,.T.);
#4144=EDGE_CURVE('',#3293,#3294,#2187,.T.);
#4145=EDGE_CURVE('',#3294,#3292,#1607,.T.);
#4146=EDGE_CURVE('',#3291,#3293,#1608,.T.);
#4147=EDGE_CURVE('',#3295,#3296,#2188,.T.);
#4148=EDGE_CURVE('',#3296,#3294,#1609,.T.);
#4149=EDGE_CURVE('',#3293,#3295,#1610,.T.);
#4150=EDGE_CURVE('',#3297,#3298,#2189,.T.);
#4151=EDGE_CURVE('',#3298,#3296,#1611,.T.);
#4152=EDGE_CURVE('',#3295,#3297,#1612,.T.);
#4153=EDGE_CURVE('',#3299,#3300,#2190,.T.);
#4154=EDGE_CURVE('',#3300,#3298,#1613,.T.);
#4155=EDGE_CURVE('',#3297,#3299,#1614,.T.);
#4156=EDGE_CURVE('',#3301,#3302,#2191,.T.);
#4157=EDGE_CURVE('',#3302,#3300,#1615,.T.);
#4158=EDGE_CURVE('',#3299,#3301,#1616,.T.);
#4159=EDGE_CURVE('',#3303,#3304,#2192,.T.);
#4160=EDGE_CURVE('',#3303,#3305,#1617,.T.);
#4161=EDGE_CURVE('',#3306,#3305,#1464,.F.);
#4162=EDGE_CURVE('',#3306,#3304,#1618,.T.);
#4163=EDGE_CURVE('',#3307,#3308,#2193,.T.);
#4164=EDGE_CURVE('',#3308,#3309,#1619,.T.);
#4165=EDGE_CURVE('',#3310,#3309,#1465,.T.);
#4166=EDGE_CURVE('',#3307,#3310,#1620,.T.);
#4167=EDGE_CURVE('',#3311,#3312,#2194,.T.);
#4168=EDGE_CURVE('',#3312,#3308,#1621,.T.);
#4169=EDGE_CURVE('',#3311,#3307,#1622,.T.);
#4170=EDGE_CURVE('',#3313,#3314,#2195,.T.);
#4171=EDGE_CURVE('',#3314,#3312,#1623,.T.);
#4172=EDGE_CURVE('',#3313,#3311,#1624,.T.);
#4173=EDGE_CURVE('',#3315,#3316,#2196,.T.);
#4174=EDGE_CURVE('',#3316,#3314,#1625,.T.);
#4175=EDGE_CURVE('',#3315,#3313,#1626,.T.);
#4176=EDGE_CURVE('',#3317,#3318,#2197,.T.);
#4177=EDGE_CURVE('',#3318,#3316,#1627,.T.);
#4178=EDGE_CURVE('',#3317,#3315,#1628,.T.);
#4179=EDGE_CURVE('',#3319,#3320,#2198,.T.);
#4180=EDGE_CURVE('',#3320,#3318,#1629,.T.);
#4181=EDGE_CURVE('',#3319,#3317,#1630,.T.);
#4182=EDGE_CURVE('',#3321,#3322,#2199,.T.);
#4183=EDGE_CURVE('',#3322,#3320,#1631,.T.);
#4184=EDGE_CURVE('',#3321,#3319,#1632,.T.);
#4185=EDGE_CURVE('',#3323,#3324,#2200,.T.);
#4186=EDGE_CURVE('',#3324,#3322,#1633,.T.);
#4187=EDGE_CURVE('',#3323,#3321,#1634,.T.);
#4188=EDGE_CURVE('',#3325,#3326,#2201,.T.);
#4189=EDGE_CURVE('',#3326,#3324,#1635,.T.);
#4190=EDGE_CURVE('',#3325,#3323,#1636,.T.);
#4191=EDGE_CURVE('',#3327,#3328,#2202,.T.);
#4192=EDGE_CURVE('',#3328,#3326,#1637,.T.);
#4193=EDGE_CURVE('',#3327,#3325,#1638,.T.);
#4194=EDGE_CURVE('',#3329,#3330,#2203,.T.);
#4195=EDGE_CURVE('',#3330,#3328,#1639,.T.);
#4196=EDGE_CURVE('',#3329,#3327,#1640,.T.);
#4197=EDGE_CURVE('',#3331,#3332,#2204,.T.);
#4198=EDGE_CURVE('',#3332,#3330,#1641,.T.);
#4199=EDGE_CURVE('',#3331,#3329,#1642,.T.);
#4200=EDGE_CURVE('',#3333,#3334,#2205,.T.);
#4201=EDGE_CURVE('',#3334,#3332,#1643,.T.);
#4202=EDGE_CURVE('',#3333,#3331,#1644,.T.);
#4203=EDGE_CURVE('',#3335,#3336,#2206,.T.);
#4204=EDGE_CURVE('',#3336,#3334,#1645,.T.);
#4205=EDGE_CURVE('',#3335,#3333,#1646,.T.);
#4206=EDGE_CURVE('',#3337,#3338,#2207,.T.);
#4207=EDGE_CURVE('',#3338,#3336,#1647,.T.);
#4208=EDGE_CURVE('',#3337,#3335,#1648,.T.);
#4209=EDGE_CURVE('',#3339,#3340,#2208,.T.);
#4210=EDGE_CURVE('',#3340,#3338,#1649,.T.);
#4211=EDGE_CURVE('',#3339,#3337,#1650,.T.);
#4212=EDGE_CURVE('',#3341,#3342,#2209,.T.);
#4213=EDGE_CURVE('',#3343,#3341,#1651,.T.);
#4214=EDGE_CURVE('',#3344,#3343,#1466,.T.);
#4215=EDGE_CURVE('',#3344,#3342,#1652,.T.);
#4216=EDGE_CURVE('',#3345,#3346,#2210,.T.);
#4217=EDGE_CURVE('',#3346,#3347,#1653,.T.);
#4218=EDGE_CURVE('',#3347,#3348,#1467,.T.);
#4219=EDGE_CURVE('',#3348,#3349,#2211,.T.);
#4220=EDGE_CURVE('',#3349,#3349,#1468,.F.);
#4221=EDGE_CURVE('',#3348,#3350,#1469,.T.);
#4222=EDGE_CURVE('',#3350,#3345,#1654,.T.);
#4223=EDGE_CURVE('',#3351,#3352,#2212,.T.);
#4224=EDGE_CURVE('',#3352,#3346,#1655,.T.);
#4225=EDGE_CURVE('',#3345,#3351,#1656,.T.);
#4226=EDGE_CURVE('',#3353,#3354,#2213,.T.);
#4227=EDGE_CURVE('',#3354,#3352,#1657,.T.);
#4228=EDGE_CURVE('',#3351,#3353,#1658,.T.);
#4229=EDGE_CURVE('',#3355,#3356,#2214,.T.);
#4230=EDGE_CURVE('',#3356,#3354,#1659,.T.);
#4231=EDGE_CURVE('',#3353,#3355,#1660,.T.);
#4232=EDGE_CURVE('',#3357,#3358,#2215,.T.);
#4233=EDGE_CURVE('',#3358,#3356,#1661,.T.);
#4234=EDGE_CURVE('',#3355,#3357,#1662,.T.);
#4235=EDGE_CURVE('',#3359,#3360,#2216,.T.);
#4236=EDGE_CURVE('',#3360,#3358,#1663,.T.);
#4237=EDGE_CURVE('',#3357,#3359,#1664,.T.);
#4238=EDGE_CURVE('',#3361,#3362,#2217,.T.);
#4239=EDGE_CURVE('',#3362,#3360,#1665,.T.);
#4240=EDGE_CURVE('',#3359,#3361,#1666,.T.);
#4241=EDGE_CURVE('',#3363,#3364,#2218,.T.);
#4242=EDGE_CURVE('',#3364,#3362,#1667,.T.);
#4243=EDGE_CURVE('',#3361,#3363,#1668,.T.);
#4244=EDGE_CURVE('',#3365,#3366,#2219,.T.);
#4245=EDGE_CURVE('',#3366,#3364,#1669,.T.);
#4246=EDGE_CURVE('',#3363,#3365,#1670,.T.);
#4247=EDGE_CURVE('',#3367,#3368,#2220,.T.);
#4248=EDGE_CURVE('',#3368,#3366,#1671,.T.);
#4249=EDGE_CURVE('',#3365,#3367,#1672,.T.);
#4250=EDGE_CURVE('',#3369,#3370,#2221,.T.);
#4251=EDGE_CURVE('',#3370,#3368,#1673,.T.);
#4252=EDGE_CURVE('',#3367,#3369,#1674,.T.);
#4253=EDGE_CURVE('',#3371,#3372,#2222,.T.);
#4254=EDGE_CURVE('',#3372,#3370,#1675,.T.);
#4255=EDGE_CURVE('',#3369,#3371,#1676,.T.);
#4256=EDGE_CURVE('',#3373,#3374,#2223,.T.);
#4257=EDGE_CURVE('',#3374,#3372,#1677,.T.);
#4258=EDGE_CURVE('',#3371,#3373,#1678,.T.);
#4259=EDGE_CURVE('',#3375,#3376,#2224,.T.);
#4260=EDGE_CURVE('',#3376,#3374,#1679,.T.);
#4261=EDGE_CURVE('',#3373,#3375,#1680,.T.);
#4262=EDGE_CURVE('',#3377,#3378,#2225,.T.);
#4263=EDGE_CURVE('',#3378,#3376,#1681,.T.);
#4264=EDGE_CURVE('',#3375,#3377,#1682,.T.);
#4265=EDGE_CURVE('',#3379,#3380,#2226,.T.);
#4266=EDGE_CURVE('',#3380,#3378,#1683,.T.);
#4267=EDGE_CURVE('',#3377,#3379,#1684,.T.);
#4268=EDGE_CURVE('',#3381,#3382,#2227,.T.);
#4269=EDGE_CURVE('',#3381,#3383,#1685,.T.);
#4270=EDGE_CURVE('',#3384,#3383,#1470,.F.);
#4271=EDGE_CURVE('',#3384,#3382,#1686,.T.);
#4272=EDGE_CURVE('',#3385,#3386,#2228,.T.);
#4273=EDGE_CURVE('',#3386,#3387,#1687,.T.);
#4274=EDGE_CURVE('',#3388,#3387,#1471,.T.);
#4275=EDGE_CURVE('',#3385,#3388,#1688,.T.);
#4276=EDGE_CURVE('',#3389,#3390,#2229,.T.);
#4277=EDGE_CURVE('',#3390,#3386,#1689,.T.);
#4278=EDGE_CURVE('',#3389,#3385,#1690,.T.);
#4279=EDGE_CURVE('',#3391,#3392,#2230,.T.);
#4280=EDGE_CURVE('',#3392,#3390,#1691,.T.);
#4281=EDGE_CURVE('',#3391,#3389,#1692,.T.);
#4282=EDGE_CURVE('',#3393,#3394,#2231,.T.);
#4283=EDGE_CURVE('',#3394,#3392,#1693,.T.);
#4284=EDGE_CURVE('',#3393,#3391,#1694,.T.);
#4285=EDGE_CURVE('',#3395,#3396,#2232,.T.);
#4286=EDGE_CURVE('',#3396,#3394,#1695,.T.);
#4287=EDGE_CURVE('',#3395,#3393,#1696,.T.);
#4288=EDGE_CURVE('',#3397,#3398,#2233,.T.);
#4289=EDGE_CURVE('',#3398,#3396,#1697,.T.);
#4290=EDGE_CURVE('',#3397,#3395,#1698,.T.);
#4291=EDGE_CURVE('',#3399,#3400,#2234,.T.);
#4292=EDGE_CURVE('',#3400,#3398,#1699,.T.);
#4293=EDGE_CURVE('',#3399,#3397,#1700,.T.);
#4294=EDGE_CURVE('',#3401,#3402,#2235,.T.);
#4295=EDGE_CURVE('',#3402,#3400,#1701,.T.);
#4296=EDGE_CURVE('',#3401,#3399,#1702,.T.);
#4297=EDGE_CURVE('',#3403,#3404,#2236,.T.);
#4298=EDGE_CURVE('',#3404,#3402,#1703,.T.);
#4299=EDGE_CURVE('',#3403,#3401,#1704,.T.);
#4300=EDGE_CURVE('',#3405,#3406,#2237,.T.);
#4301=EDGE_CURVE('',#3406,#3404,#1705,.T.);
#4302=EDGE_CURVE('',#3405,#3403,#1706,.T.);
#4303=EDGE_CURVE('',#3407,#3408,#2238,.T.);
#4304=EDGE_CURVE('',#3408,#3406,#1707,.T.);
#4305=EDGE_CURVE('',#3407,#3405,#1708,.T.);
#4306=EDGE_CURVE('',#3409,#3410,#2239,.T.);
#4307=EDGE_CURVE('',#3410,#3408,#1709,.T.);
#4308=EDGE_CURVE('',#3409,#3407,#1710,.T.);
#4309=EDGE_CURVE('',#3411,#3412,#2240,.T.);
#4310=EDGE_CURVE('',#3412,#3410,#1711,.T.);
#4311=EDGE_CURVE('',#3411,#3409,#1712,.T.);
#4312=EDGE_CURVE('',#3413,#3414,#2241,.T.);
#4313=EDGE_CURVE('',#3414,#3412,#1713,.T.);
#4314=EDGE_CURVE('',#3413,#3411,#1714,.T.);
#4315=EDGE_CURVE('',#3415,#3416,#2242,.T.);
#4316=EDGE_CURVE('',#3416,#3414,#1715,.T.);
#4317=EDGE_CURVE('',#3415,#3413,#1716,.T.);
#4318=EDGE_CURVE('',#3417,#3418,#2243,.T.);
#4319=EDGE_CURVE('',#3418,#3416,#1717,.T.);
#4320=EDGE_CURVE('',#3417,#3415,#1718,.T.);
#4321=EDGE_CURVE('',#3419,#3420,#2244,.T.);
#4322=EDGE_CURVE('',#3421,#3419,#1719,.T.);
#4323=EDGE_CURVE('',#3422,#3421,#1472,.T.);
#4324=EDGE_CURVE('',#3422,#3420,#1720,.T.);
#4325=EDGE_CURVE('',#3423,#3424,#2245,.T.);
#4326=EDGE_CURVE('',#3424,#3425,#1721,.T.);
#4327=EDGE_CURVE('',#3425,#3426,#1473,.T.);
#4328=EDGE_CURVE('',#3426,#3427,#2246,.T.);
#4329=EDGE_CURVE('',#3427,#3427,#1474,.F.);
#4330=EDGE_CURVE('',#3426,#3428,#1475,.T.);
#4331=EDGE_CURVE('',#3428,#3423,#1722,.T.);
#4332=EDGE_CURVE('',#3429,#3430,#2247,.T.);
#4333=EDGE_CURVE('',#3430,#3424,#1723,.T.);
#4334=EDGE_CURVE('',#3423,#3429,#1724,.T.);
#4335=EDGE_CURVE('',#3431,#3432,#2248,.T.);
#4336=EDGE_CURVE('',#3432,#3430,#1725,.T.);
#4337=EDGE_CURVE('',#3429,#3431,#1726,.T.);
#4338=EDGE_CURVE('',#3433,#3434,#2249,.T.);
#4339=EDGE_CURVE('',#3434,#3432,#1727,.T.);
#4340=EDGE_CURVE('',#3431,#3433,#1728,.T.);
#4341=EDGE_CURVE('',#3435,#3436,#2250,.T.);
#4342=EDGE_CURVE('',#3436,#3434,#1729,.T.);
#4343=EDGE_CURVE('',#3433,#3435,#1730,.T.);
#4344=EDGE_CURVE('',#3437,#3438,#2251,.T.);
#4345=EDGE_CURVE('',#3438,#3436,#1731,.T.);
#4346=EDGE_CURVE('',#3435,#3437,#1732,.T.);
#4347=EDGE_CURVE('',#3439,#3440,#2252,.T.);
#4348=EDGE_CURVE('',#3440,#3438,#1733,.T.);
#4349=EDGE_CURVE('',#3437,#3439,#1734,.T.);
#4350=EDGE_CURVE('',#3441,#3442,#2253,.T.);
#4351=EDGE_CURVE('',#3442,#3440,#1735,.T.);
#4352=EDGE_CURVE('',#3439,#3441,#1736,.T.);
#4353=EDGE_CURVE('',#3443,#3444,#2254,.T.);
#4354=EDGE_CURVE('',#3444,#3442,#1737,.T.);
#4355=EDGE_CURVE('',#3441,#3443,#1738,.T.);
#4356=EDGE_CURVE('',#3445,#3446,#2255,.T.);
#4357=EDGE_CURVE('',#3446,#3444,#1739,.T.);
#4358=EDGE_CURVE('',#3443,#3445,#1740,.T.);
#4359=EDGE_CURVE('',#3447,#3448,#2256,.T.);
#4360=EDGE_CURVE('',#3448,#3446,#1741,.T.);
#4361=EDGE_CURVE('',#3445,#3447,#1742,.T.);
#4362=EDGE_CURVE('',#3449,#3450,#2257,.T.);
#4363=EDGE_CURVE('',#3450,#3448,#1743,.T.);
#4364=EDGE_CURVE('',#3447,#3449,#1744,.T.);
#4365=EDGE_CURVE('',#3451,#3452,#2258,.T.);
#4366=EDGE_CURVE('',#3452,#3450,#1745,.T.);
#4367=EDGE_CURVE('',#3449,#3451,#1746,.T.);
#4368=EDGE_CURVE('',#3453,#3454,#2259,.T.);
#4369=EDGE_CURVE('',#3454,#3452,#1747,.T.);
#4370=EDGE_CURVE('',#3451,#3453,#1748,.T.);
#4371=EDGE_CURVE('',#3455,#3456,#2260,.T.);
#4372=EDGE_CURVE('',#3456,#3454,#1749,.T.);
#4373=EDGE_CURVE('',#3453,#3455,#1750,.T.);
#4374=EDGE_CURVE('',#3457,#3458,#2261,.T.);
#4375=EDGE_CURVE('',#3458,#3456,#1751,.T.);
#4376=EDGE_CURVE('',#3455,#3457,#1752,.T.);
#4377=EDGE_CURVE('',#3459,#3460,#2262,.T.);
#4378=EDGE_CURVE('',#3459,#3461,#1753,.T.);
#4379=EDGE_CURVE('',#3462,#3461,#1476,.F.);
#4380=EDGE_CURVE('',#3462,#3460,#1754,.T.);
#4381=EDGE_CURVE('',#3463,#3464,#2263,.T.);
#4382=EDGE_CURVE('',#3464,#3465,#1755,.T.);
#4383=EDGE_CURVE('',#3466,#3465,#1477,.T.);
#4384=EDGE_CURVE('',#3463,#3466,#1756,.T.);
#4385=EDGE_CURVE('',#3467,#3468,#2264,.T.);
#4386=EDGE_CURVE('',#3468,#3464,#1757,.T.);
#4387=EDGE_CURVE('',#3467,#3463,#1758,.T.);
#4388=EDGE_CURVE('',#3469,#3470,#2265,.T.);
#4389=EDGE_CURVE('',#3470,#3468,#1759,.T.);
#4390=EDGE_CURVE('',#3469,#3467,#1760,.T.);
#4391=EDGE_CURVE('',#3471,#3472,#2266,.T.);
#4392=EDGE_CURVE('',#3472,#3470,#1761,.T.);
#4393=EDGE_CURVE('',#3471,#3469,#1762,.T.);
#4394=EDGE_CURVE('',#3473,#3474,#2267,.T.);
#4395=EDGE_CURVE('',#3474,#3472,#1763,.T.);
#4396=EDGE_CURVE('',#3473,#3471,#1764,.T.);
#4397=EDGE_CURVE('',#3475,#3476,#2268,.T.);
#4398=EDGE_CURVE('',#3476,#3474,#1765,.T.);
#4399=EDGE_CURVE('',#3475,#3473,#1766,.T.);
#4400=EDGE_CURVE('',#3477,#3478,#2269,.T.);
#4401=EDGE_CURVE('',#3478,#3476,#1767,.T.);
#4402=EDGE_CURVE('',#3477,#3475,#1768,.T.);
#4403=EDGE_CURVE('',#3479,#3480,#2270,.T.);
#4404=EDGE_CURVE('',#3480,#3478,#1769,.T.);
#4405=EDGE_CURVE('',#3479,#3477,#1770,.T.);
#4406=EDGE_CURVE('',#3481,#3482,#2271,.T.);
#4407=EDGE_CURVE('',#3482,#3480,#1771,.T.);
#4408=EDGE_CURVE('',#3481,#3479,#1772,.T.);
#4409=EDGE_CURVE('',#3483,#3484,#2272,.T.);
#4410=EDGE_CURVE('',#3484,#3482,#1773,.T.);
#4411=EDGE_CURVE('',#3483,#3481,#1774,.T.);
#4412=EDGE_CURVE('',#3485,#3486,#2273,.T.);
#4413=EDGE_CURVE('',#3486,#3484,#1775,.T.);
#4414=EDGE_CURVE('',#3485,#3483,#1776,.T.);
#4415=EDGE_CURVE('',#3487,#3488,#2274,.T.);
#4416=EDGE_CURVE('',#3488,#3486,#1777,.T.);
#4417=EDGE_CURVE('',#3487,#3485,#1778,.T.);
#4418=EDGE_CURVE('',#3489,#3490,#2275,.T.);
#4419=EDGE_CURVE('',#3490,#3488,#1779,.T.);
#4420=EDGE_CURVE('',#3489,#3487,#1780,.T.);
#4421=EDGE_CURVE('',#3491,#3492,#2276,.T.);
#4422=EDGE_CURVE('',#3492,#3490,#1781,.T.);
#4423=EDGE_CURVE('',#3491,#3489,#1782,.T.);
#4424=EDGE_CURVE('',#3493,#3494,#2277,.T.);
#4425=EDGE_CURVE('',#3494,#3492,#1783,.T.);
#4426=EDGE_CURVE('',#3493,#3491,#1784,.T.);
#4427=EDGE_CURVE('',#3495,#3496,#2278,.T.);
#4428=EDGE_CURVE('',#3496,#3494,#1785,.T.);
#4429=EDGE_CURVE('',#3495,#3493,#1786,.T.);
#4430=EDGE_CURVE('',#3497,#3498,#2279,.T.);
#4431=EDGE_CURVE('',#3499,#3497,#1787,.T.);
#4432=EDGE_CURVE('',#3500,#3499,#1478,.T.);
#4433=EDGE_CURVE('',#3500,#3498,#1788,.T.);
#4434=EDGE_CURVE('',#3501,#3502,#2280,.T.);
#4435=EDGE_CURVE('',#3502,#3503,#1789,.T.);
#4436=EDGE_CURVE('',#3503,#3504,#1479,.T.);
#4437=EDGE_CURVE('',#3504,#3505,#2281,.T.);
#4438=EDGE_CURVE('',#3505,#3505,#1480,.F.);
#4439=EDGE_CURVE('',#3504,#3506,#1481,.T.);
#4440=EDGE_CURVE('',#3506,#3501,#1790,.T.);
#4441=EDGE_CURVE('',#3507,#3508,#2282,.T.);
#4442=EDGE_CURVE('',#3508,#3502,#1791,.T.);
#4443=EDGE_CURVE('',#3501,#3507,#1792,.T.);
#4444=EDGE_CURVE('',#3509,#3510,#2283,.T.);
#4445=EDGE_CURVE('',#3510,#3508,#1793,.T.);
#4446=EDGE_CURVE('',#3507,#3509,#1794,.T.);
#4447=EDGE_CURVE('',#3511,#3512,#2284,.T.);
#4448=EDGE_CURVE('',#3512,#3510,#1795,.T.);
#4449=EDGE_CURVE('',#3509,#3511,#1796,.T.);
#4450=EDGE_CURVE('',#3513,#3514,#2285,.T.);
#4451=EDGE_CURVE('',#3514,#3512,#1797,.T.);
#4452=EDGE_CURVE('',#3511,#3513,#1798,.T.);
#4453=EDGE_CURVE('',#3515,#3516,#2286,.T.);
#4454=EDGE_CURVE('',#3516,#3514,#1799,.T.);
#4455=EDGE_CURVE('',#3513,#3515,#1800,.T.);
#4456=EDGE_CURVE('',#3517,#3518,#2287,.T.);
#4457=EDGE_CURVE('',#3518,#3516,#1801,.T.);
#4458=EDGE_CURVE('',#3515,#3517,#1802,.T.);
#4459=EDGE_CURVE('',#3519,#3520,#2288,.T.);
#4460=EDGE_CURVE('',#3520,#3518,#1803,.T.);
#4461=EDGE_CURVE('',#3517,#3519,#1804,.T.);
#4462=EDGE_CURVE('',#3521,#3522,#2289,.T.);
#4463=EDGE_CURVE('',#3522,#3520,#1805,.T.);
#4464=EDGE_CURVE('',#3519,#3521,#1806,.T.);
#4465=EDGE_CURVE('',#3523,#3524,#2290,.T.);
#4466=EDGE_CURVE('',#3524,#3522,#1807,.T.);
#4467=EDGE_CURVE('',#3521,#3523,#1808,.T.);
#4468=EDGE_CURVE('',#3525,#3526,#2291,.T.);
#4469=EDGE_CURVE('',#3526,#3524,#1809,.T.);
#4470=EDGE_CURVE('',#3523,#3525,#1810,.T.);
#4471=EDGE_CURVE('',#3527,#3528,#2292,.T.);
#4472=EDGE_CURVE('',#3528,#3526,#1811,.T.);
#4473=EDGE_CURVE('',#3525,#3527,#1812,.T.);
#4474=EDGE_CURVE('',#3529,#3530,#2293,.T.);
#4475=EDGE_CURVE('',#3530,#3528,#1813,.T.);
#4476=EDGE_CURVE('',#3527,#3529,#1814,.T.);
#4477=EDGE_CURVE('',#3531,#3532,#2294,.T.);
#4478=EDGE_CURVE('',#3532,#3530,#1815,.T.);
#4479=EDGE_CURVE('',#3529,#3531,#1816,.T.);
#4480=EDGE_CURVE('',#3533,#3534,#2295,.T.);
#4481=EDGE_CURVE('',#3534,#3532,#1817,.T.);
#4482=EDGE_CURVE('',#3531,#3533,#1818,.T.);
#4483=EDGE_CURVE('',#3535,#3536,#2296,.T.);
#4484=EDGE_CURVE('',#3536,#3534,#1819,.T.);
#4485=EDGE_CURVE('',#3533,#3535,#1820,.T.);
#4486=EDGE_CURVE('',#3537,#3538,#2297,.T.);
#4487=EDGE_CURVE('',#3537,#3539,#1821,.T.);
#4488=EDGE_CURVE('',#3540,#3539,#1482,.F.);
#4489=EDGE_CURVE('',#3540,#3538,#1822,.T.);
#4490=EDGE_CURVE('',#3541,#3542,#2298,.T.);
#4491=EDGE_CURVE('',#3542,#3543,#1823,.T.);
#4492=EDGE_CURVE('',#3544,#3543,#1483,.T.);
#4493=EDGE_CURVE('',#3541,#3544,#1824,.T.);
#4494=EDGE_CURVE('',#3545,#3546,#2299,.T.);
#4495=EDGE_CURVE('',#3546,#3542,#1825,.T.);
#4496=EDGE_CURVE('',#3545,#3541,#1826,.T.);
#4497=EDGE_CURVE('',#3547,#3548,#2300,.T.);
#4498=EDGE_CURVE('',#3548,#3546,#1827,.T.);
#4499=EDGE_CURVE('',#3547,#3545,#1828,.T.);
#4500=EDGE_CURVE('',#3549,#3550,#2301,.T.);
#4501=EDGE_CURVE('',#3550,#3548,#1829,.T.);
#4502=EDGE_CURVE('',#3549,#3547,#1830,.T.);
#4503=EDGE_CURVE('',#3551,#3552,#2302,.T.);
#4504=EDGE_CURVE('',#3552,#3550,#1831,.T.);
#4505=EDGE_CURVE('',#3551,#3549,#1832,.T.);
#4506=EDGE_CURVE('',#3553,#3554,#2303,.T.);
#4507=EDGE_CURVE('',#3554,#3552,#1833,.T.);
#4508=EDGE_CURVE('',#3553,#3551,#1834,.T.);
#4509=EDGE_CURVE('',#3555,#3556,#2304,.T.);
#4510=EDGE_CURVE('',#3556,#3554,#1835,.T.);
#4511=EDGE_CURVE('',#3555,#3553,#1836,.T.);
#4512=EDGE_CURVE('',#3557,#3558,#2305,.T.);
#4513=EDGE_CURVE('',#3558,#3556,#1837,.T.);
#4514=EDGE_CURVE('',#3557,#3555,#1838,.T.);
#4515=EDGE_CURVE('',#3559,#3560,#2306,.T.);
#4516=EDGE_CURVE('',#3560,#3558,#1839,.T.);
#4517=EDGE_CURVE('',#3559,#3557,#1840,.T.);
#4518=EDGE_CURVE('',#3561,#3562,#2307,.T.);
#4519=EDGE_CURVE('',#3562,#3560,#1841,.T.);
#4520=EDGE_CURVE('',#3561,#3559,#1842,.T.);
#4521=EDGE_CURVE('',#3563,#3564,#2308,.T.);
#4522=EDGE_CURVE('',#3564,#3562,#1843,.T.);
#4523=EDGE_CURVE('',#3563,#3561,#1844,.T.);
#4524=EDGE_CURVE('',#3565,#3566,#2309,.T.);
#4525=EDGE_CURVE('',#3566,#3564,#1845,.T.);
#4526=EDGE_CURVE('',#3565,#3563,#1846,.T.);
#4527=EDGE_CURVE('',#3567,#3568,#2310,.T.);
#4528=EDGE_CURVE('',#3568,#3566,#1847,.T.);
#4529=EDGE_CURVE('',#3567,#3565,#1848,.T.);
#4530=EDGE_CURVE('',#3569,#3570,#2311,.T.);
#4531=EDGE_CURVE('',#3570,#3568,#1849,.T.);
#4532=EDGE_CURVE('',#3569,#3567,#1850,.T.);
#4533=EDGE_CURVE('',#3571,#3572,#2312,.T.);
#4534=EDGE_CURVE('',#3572,#3570,#1851,.T.);
#4535=EDGE_CURVE('',#3571,#3569,#1852,.T.);
#4536=EDGE_CURVE('',#3573,#3574,#2313,.T.);
#4537=EDGE_CURVE('',#3574,#3572,#1853,.T.);
#4538=EDGE_CURVE('',#3573,#3571,#1854,.T.);
#4539=EDGE_CURVE('',#3575,#3576,#2314,.T.);
#4540=EDGE_CURVE('',#3577,#3575,#1855,.T.);
#4541=EDGE_CURVE('',#3578,#3577,#1484,.T.);
#4542=EDGE_CURVE('',#3578,#3576,#1856,.T.);
#4543=EDGE_CURVE('',#3503,#3544,#1857,.T.);
#4544=EDGE_CURVE('',#3543,#3506,#1858,.T.);
#4545=EDGE_CURVE('',#3576,#3574,#1859,.T.);
#4546=EDGE_CURVE('',#3575,#3573,#1860,.T.);
#4547=EDGE_CURVE('',#3539,#3578,#1861,.T.);
#4548=EDGE_CURVE('',#3535,#3537,#1862,.T.);
#4549=EDGE_CURVE('',#3538,#3536,#1863,.T.);
#4550=EDGE_CURVE('',#3577,#3540,#1864,.T.);
#4551=EDGE_CURVE('',#3425,#3466,#1865,.T.);
#4552=EDGE_CURVE('',#3465,#3428,#1866,.T.);
#4553=EDGE_CURVE('',#3498,#3496,#1867,.T.);
#4554=EDGE_CURVE('',#3497,#3495,#1868,.T.);
#4555=EDGE_CURVE('',#3461,#3500,#1869,.T.);
#4556=EDGE_CURVE('',#3457,#3459,#1870,.T.);
#4557=EDGE_CURVE('',#3460,#3458,#1871,.T.);
#4558=EDGE_CURVE('',#3499,#3462,#1872,.T.);
#4559=EDGE_CURVE('',#3347,#3388,#1873,.T.);
#4560=EDGE_CURVE('',#3387,#3350,#1874,.T.);
#4561=EDGE_CURVE('',#3420,#3418,#1875,.T.);
#4562=EDGE_CURVE('',#3419,#3417,#1876,.T.);
#4563=EDGE_CURVE('',#3383,#3422,#1877,.T.);
#4564=EDGE_CURVE('',#3379,#3381,#1878,.T.);
#4565=EDGE_CURVE('',#3382,#3380,#1879,.T.);
#4566=EDGE_CURVE('',#3421,#3384,#1880,.T.);
#4567=EDGE_CURVE('',#3269,#3310,#1881,.T.);
#4568=EDGE_CURVE('',#3309,#3272,#1882,.T.);
#4569=EDGE_CURVE('',#3342,#3340,#1883,.T.);
#4570=EDGE_CURVE('',#3341,#3339,#1884,.T.);
#4571=EDGE_CURVE('',#3305,#3344,#1885,.T.);
#4572=EDGE_CURVE('',#3301,#3303,#1886,.T.);
#4573=EDGE_CURVE('',#3304,#3302,#1887,.T.);
#4574=EDGE_CURVE('',#3343,#3306,#1888,.T.);
#4575=EDGE_CURVE('',#3579,#3580,#2315,.T.);
#4576=EDGE_CURVE('',#3580,#3581,#2316,.T.);
#4577=EDGE_CURVE('',#3582,#3581,#2317,.T.);
#4578=EDGE_CURVE('',#3579,#3582,#2318,.T.);
#4579=EDGE_CURVE('',#3583,#3579,#2319,.T.);
#4580=EDGE_CURVE('',#3584,#3582,#2320,.T.);
#4581=EDGE_CURVE('',#3583,#3584,#2321,.T.);
#4582=EDGE_CURVE('',#3585,#3583,#2322,.T.);
#4583=EDGE_CURVE('',#3586,#3584,#2323,.T.);
#4584=EDGE_CURVE('',#3585,#3586,#2324,.T.);
#4585=EDGE_CURVE('',#3580,#3585,#2325,.T.);
#4586=EDGE_CURVE('',#3581,#3586,#2326,.T.);
#4587=EDGE_CURVE('',#3587,#3588,#2327,.F.);
#4588=EDGE_CURVE('',#3588,#3589,#2328,.T.);
#4589=EDGE_CURVE('',#3590,#3589,#2329,.F.);
#4590=EDGE_CURVE('',#3587,#3590,#2330,.F.);
#4591=EDGE_CURVE('',#3591,#3587,#2331,.F.);
#4592=EDGE_CURVE('',#3592,#3590,#2332,.F.);
#4593=EDGE_CURVE('',#3591,#3592,#2333,.F.);
#4594=EDGE_CURVE('',#3593,#3591,#2334,.F.);
#4595=EDGE_CURVE('',#3594,#3592,#2335,.F.);
#4596=EDGE_CURVE('',#3593,#3594,#2336,.T.);
#4597=EDGE_CURVE('',#3588,#3593,#2337,.F.);
#4598=EDGE_CURVE('',#3589,#3594,#2338,.F.);
#4599=EDGE_CURVE('',#3595,#3595,#1485,.T.);
#4600=EDGE_CURVE('',#3595,#3596,#2339,.T.);
#4601=EDGE_CURVE('',#3596,#3596,#1486,.T.);
#4602=EDGE_CURVE('',#3597,#3597,#1487,.T.);
#4603=EDGE_CURVE('',#3597,#3598,#2340,.T.);
#4604=EDGE_CURVE('',#3598,#3598,#1488,.T.);
#4605=EDGE_CURVE('',#3599,#3599,#1489,.T.);
#4606=EDGE_CURVE('',#3599,#3600,#2341,.T.);
#4607=EDGE_CURVE('',#3600,#3600,#1490,.T.);
#4608=EDGE_CURVE('',#3601,#3601,#1491,.T.);
#4609=EDGE_CURVE('',#3601,#3602,#2342,.T.);
#4610=EDGE_CURVE('',#3602,#3602,#1492,.T.);
#4611=EDGE_CURVE('',#3603,#3603,#1493,.T.);
#4612=EDGE_CURVE('',#3603,#3604,#2343,.T.);
#4613=EDGE_CURVE('',#3604,#3604,#1494,.T.);
#4614=EDGE_CURVE('',#3605,#3606,#2344,.T.);
#4615=EDGE_CURVE('',#3606,#3607,#2345,.T.);
#4616=EDGE_CURVE('',#3608,#3607,#2346,.T.);
#4617=EDGE_CURVE('',#3605,#3608,#2347,.T.);
#4618=EDGE_CURVE('',#3609,#3605,#2348,.T.);
#4619=EDGE_CURVE('',#3610,#3608,#2349,.T.);
#4620=EDGE_CURVE('',#3609,#3610,#2350,.T.);
#4621=EDGE_CURVE('',#3611,#3609,#2351,.T.);
#4622=EDGE_CURVE('',#3612,#3610,#2352,.T.);
#4623=EDGE_CURVE('',#3611,#3612,#2353,.T.);
#4624=EDGE_CURVE('',#3606,#3611,#2354,.T.);
#4625=EDGE_CURVE('',#3607,#3612,#2355,.T.);
#4626=EDGE_CURVE('',#3613,#3614,#2356,.T.);
#4627=EDGE_CURVE('',#3614,#3615,#2357,.T.);
#4628=EDGE_CURVE('',#3616,#3615,#2358,.T.);
#4629=EDGE_CURVE('',#3613,#3616,#2359,.T.);
#4630=EDGE_CURVE('',#3617,#3613,#2360,.T.);
#4631=EDGE_CURVE('',#3618,#3616,#2361,.T.);
#4632=EDGE_CURVE('',#3617,#3618,#2362,.T.);
#4633=EDGE_CURVE('',#3619,#3617,#2363,.T.);
#4634=EDGE_CURVE('',#3620,#3618,#2364,.T.);
#4635=EDGE_CURVE('',#3619,#3620,#2365,.T.);
#4636=EDGE_CURVE('',#3614,#3619,#2366,.T.);
#4637=EDGE_CURVE('',#3615,#3620,#2367,.T.);
#4638=EDGE_CURVE('',#3621,#3622,#2368,.T.);
#4639=EDGE_CURVE('',#3622,#3623,#2369,.T.);
#4640=EDGE_CURVE('',#3624,#3623,#2370,.T.);
#4641=EDGE_CURVE('',#3621,#3624,#2371,.T.);
#4642=EDGE_CURVE('',#3625,#3621,#2372,.T.);
#4643=EDGE_CURVE('',#3626,#3624,#2373,.T.);
#4644=EDGE_CURVE('',#3625,#3626,#2374,.T.);
#4645=EDGE_CURVE('',#3627,#3625,#2375,.T.);
#4646=EDGE_CURVE('',#3628,#3626,#2376,.T.);
#4647=EDGE_CURVE('',#3627,#3628,#2377,.T.);
#4648=EDGE_CURVE('',#3622,#3627,#2378,.T.);
#4649=EDGE_CURVE('',#3623,#3628,#2379,.T.);
#4650=EDGE_CURVE('',#3629,#3630,#2380,.T.);
#4651=EDGE_CURVE('',#3630,#3631,#1889,.T.);
#4652=EDGE_CURVE('',#3631,#3632,#1495,.T.);
#4653=EDGE_CURVE('',#3632,#3633,#1890,.T.);
#4654=EDGE_CURVE('',#3633,#3634,#2381,.T.);
#4655=EDGE_CURVE('',#3634,#3634,#1496,.F.);
#4656=EDGE_CURVE('',#3633,#3629,#1891,.T.);
#4657=EDGE_CURVE('',#3635,#3636,#2382,.T.);
#4658=EDGE_CURVE('',#3636,#3630,#1892,.T.);
#4659=EDGE_CURVE('',#3629,#3635,#1893,.T.);
#4660=EDGE_CURVE('',#3637,#3638,#2383,.T.);
#4661=EDGE_CURVE('',#3638,#3636,#1894,.T.);
#4662=EDGE_CURVE('',#3635,#3637,#1895,.T.);
#4663=EDGE_CURVE('',#3639,#3640,#2384,.T.);
#4664=EDGE_CURVE('',#3640,#3638,#1896,.T.);
#4665=EDGE_CURVE('',#3637,#3639,#1897,.T.);
#4666=EDGE_CURVE('',#3641,#3642,#2385,.T.);
#4667=EDGE_CURVE('',#3642,#3640,#1898,.T.);
#4668=EDGE_CURVE('',#3639,#3641,#1899,.T.);
#4669=EDGE_CURVE('',#3643,#3644,#2386,.T.);
#4670=EDGE_CURVE('',#3644,#3642,#1900,.T.);
#4671=EDGE_CURVE('',#3641,#3643,#1901,.T.);
#4672=EDGE_CURVE('',#3645,#3646,#2387,.T.);
#4673=EDGE_CURVE('',#3646,#3644,#1902,.T.);
#4674=EDGE_CURVE('',#3643,#3645,#1903,.T.);
#4675=EDGE_CURVE('',#3647,#3648,#2388,.T.);
#4676=EDGE_CURVE('',#3648,#3646,#1904,.T.);
#4677=EDGE_CURVE('',#3645,#3647,#1905,.T.);
#4678=EDGE_CURVE('',#3649,#3650,#2389,.T.);
#4679=EDGE_CURVE('',#3650,#3648,#1906,.T.);
#4680=EDGE_CURVE('',#3647,#3649,#1907,.T.);
#4681=EDGE_CURVE('',#3651,#3652,#2390,.T.);
#4682=EDGE_CURVE('',#3652,#3650,#1908,.T.);
#4683=EDGE_CURVE('',#3649,#3651,#1909,.T.);
#4684=EDGE_CURVE('',#3653,#3654,#2391,.T.);
#4685=EDGE_CURVE('',#3654,#3652,#1910,.T.);
#4686=EDGE_CURVE('',#3651,#3653,#1911,.T.);
#4687=EDGE_CURVE('',#3655,#3656,#2392,.T.);
#4688=EDGE_CURVE('',#3656,#3654,#1912,.T.);
#4689=EDGE_CURVE('',#3653,#3655,#1913,.T.);
#4690=EDGE_CURVE('',#3657,#3658,#2393,.T.);
#4691=EDGE_CURVE('',#3658,#3656,#1914,.T.);
#4692=EDGE_CURVE('',#3655,#3657,#1915,.T.);
#4693=EDGE_CURVE('',#3659,#3660,#2394,.T.);
#4694=EDGE_CURVE('',#3660,#3658,#1916,.T.);
#4695=EDGE_CURVE('',#3657,#3659,#1917,.T.);
#4696=EDGE_CURVE('',#3661,#3662,#2395,.T.);
#4697=EDGE_CURVE('',#3661,#3663,#1918,.T.);
#4698=EDGE_CURVE('',#3664,#3663,#1497,.T.);
#4699=EDGE_CURVE('',#3664,#3662,#1919,.T.);
#4700=EDGE_CURVE('',#3665,#3666,#2396,.T.);
#4701=EDGE_CURVE('',#3666,#3667,#1920,.T.);
#4702=EDGE_CURVE('',#3668,#3667,#1498,.T.);
#4703=EDGE_CURVE('',#3665,#3668,#1921,.T.);
#4704=EDGE_CURVE('',#3669,#3670,#2397,.T.);
#4705=EDGE_CURVE('',#3670,#3666,#1922,.T.);
#4706=EDGE_CURVE('',#3669,#3665,#1923,.T.);
#4707=EDGE_CURVE('',#3671,#3672,#2398,.T.);
#4708=EDGE_CURVE('',#3672,#3670,#1924,.T.);
#4709=EDGE_CURVE('',#3671,#3669,#1925,.T.);
#4710=EDGE_CURVE('',#3673,#3674,#2399,.T.);
#4711=EDGE_CURVE('',#3674,#3672,#1926,.T.);
#4712=EDGE_CURVE('',#3673,#3671,#1927,.T.);
#4713=EDGE_CURVE('',#3675,#3676,#2400,.T.);
#4714=EDGE_CURVE('',#3676,#3674,#1928,.T.);
#4715=EDGE_CURVE('',#3675,#3673,#1929,.T.);
#4716=EDGE_CURVE('',#3677,#3678,#2401,.T.);
#4717=EDGE_CURVE('',#3678,#3676,#1930,.T.);
#4718=EDGE_CURVE('',#3677,#3675,#1931,.T.);
#4719=EDGE_CURVE('',#3679,#3680,#2402,.T.);
#4720=EDGE_CURVE('',#3680,#3678,#1932,.T.);
#4721=EDGE_CURVE('',#3679,#3677,#1933,.T.);
#4722=EDGE_CURVE('',#3681,#3682,#2403,.T.);
#4723=EDGE_CURVE('',#3682,#3680,#1934,.T.);
#4724=EDGE_CURVE('',#3681,#3679,#1935,.T.);
#4725=EDGE_CURVE('',#3683,#3684,#2404,.T.);
#4726=EDGE_CURVE('',#3684,#3682,#1936,.T.);
#4727=EDGE_CURVE('',#3683,#3681,#1937,.T.);
#4728=EDGE_CURVE('',#3685,#3686,#2405,.T.);
#4729=EDGE_CURVE('',#3686,#3684,#1938,.T.);
#4730=EDGE_CURVE('',#3685,#3683,#1939,.T.);
#4731=EDGE_CURVE('',#3687,#3688,#2406,.T.);
#4732=EDGE_CURVE('',#3688,#3686,#1940,.T.);
#4733=EDGE_CURVE('',#3687,#3685,#1941,.T.);
#4734=EDGE_CURVE('',#3689,#3690,#2407,.T.);
#4735=EDGE_CURVE('',#3690,#3688,#1942,.T.);
#4736=EDGE_CURVE('',#3689,#3687,#1943,.T.);
#4737=EDGE_CURVE('',#3691,#3692,#2408,.T.);
#4738=EDGE_CURVE('',#3692,#3690,#1944,.T.);
#4739=EDGE_CURVE('',#3691,#3689,#1945,.T.);
#4740=EDGE_CURVE('',#3693,#3694,#2409,.T.);
#4741=EDGE_CURVE('',#3694,#3692,#1946,.T.);
#4742=EDGE_CURVE('',#3693,#3691,#1947,.T.);
#4743=EDGE_CURVE('',#3695,#3696,#2410,.T.);
#4744=EDGE_CURVE('',#3696,#3694,#1948,.T.);
#4745=EDGE_CURVE('',#3695,#3693,#1949,.T.);
#4746=EDGE_CURVE('',#3697,#3698,#2411,.T.);
#4747=EDGE_CURVE('',#3699,#3697,#1950,.T.);
#4748=EDGE_CURVE('',#3700,#3699,#1499,.T.);
#4749=EDGE_CURVE('',#3700,#3698,#1951,.T.);
#4750=EDGE_CURVE('',#3631,#3668,#1952,.T.);
#4751=EDGE_CURVE('',#3667,#3632,#1953,.T.);
#4752=EDGE_CURVE('',#3698,#3696,#1954,.T.);
#4753=EDGE_CURVE('',#3697,#3695,#1955,.T.);
#4754=EDGE_CURVE('',#3663,#3700,#1956,.T.);
#4755=EDGE_CURVE('',#3659,#3661,#1957,.T.);
#4756=EDGE_CURVE('',#3662,#3660,#1958,.T.);
#4757=EDGE_CURVE('',#3699,#3664,#1959,.T.);
#4758=EDGE_CURVE('',#3701,#3702,#2412,.T.);
#4759=EDGE_CURVE('',#3702,#3703,#2413,.T.);
#4760=EDGE_CURVE('',#3704,#3703,#2414,.T.);
#4761=EDGE_CURVE('',#3701,#3704,#2415,.T.);
#4762=EDGE_CURVE('',#3702,#3705,#2416,.T.);
#4763=EDGE_CURVE('',#3705,#3706,#2417,.T.);
#4764=EDGE_CURVE('',#3703,#3706,#2418,.T.);
#4765=EDGE_CURVE('',#3705,#3707,#2419,.T.);
#4766=EDGE_CURVE('',#3707,#3708,#2420,.T.);
#4767=EDGE_CURVE('',#3706,#3708,#2421,.T.);
#4768=EDGE_CURVE('',#3707,#3701,#2422,.T.);
#4769=EDGE_CURVE('',#3708,#3704,#2423,.T.);
#4770=EDGE_CURVE('',#3709,#3709,#1500,.T.);
#4771=EDGE_CURVE('',#3709,#3710,#2424,.T.);
#4772=EDGE_CURVE('',#3710,#3710,#1501,.T.);
#4773=EDGE_CURVE('',#3711,#3711,#1502,.T.);
#4774=EDGE_CURVE('',#3712,#3712,#1503,.T.);
#4775=EDGE_CURVE('',#3713,#3713,#1504,.T.);
#4776=EDGE_CURVE('',#3713,#3712,#2425,.T.);
#4777=EDGE_CURVE('',#3714,#3715,#2426,.T.);
#4778=EDGE_CURVE('',#3714,#3716,#2427,.T.);
#4779=EDGE_CURVE('',#3717,#3716,#2428,.T.);
#4780=EDGE_CURVE('',#3715,#3717,#2429,.T.);
#4781=EDGE_CURVE('',#3715,#3718,#2430,.T.);
#4782=EDGE_CURVE('',#3719,#3717,#2431,.T.);
#4783=EDGE_CURVE('',#3718,#3719,#2432,.T.);
#4784=EDGE_CURVE('',#3718,#3720,#2433,.T.);
#4785=EDGE_CURVE('',#3721,#3719,#2434,.T.);
#4786=EDGE_CURVE('',#3720,#3721,#2435,.T.);
#4787=EDGE_CURVE('',#3720,#3722,#2436,.T.);
#4788=EDGE_CURVE('',#3723,#3721,#2437,.T.);
#4789=EDGE_CURVE('',#3722,#3723,#2438,.T.);
#4790=EDGE_CURVE('',#3722,#3724,#2439,.T.);
#4791=EDGE_CURVE('',#3725,#3723,#2440,.T.);
#4792=EDGE_CURVE('',#3724,#3725,#2441,.T.);
#4793=EDGE_CURVE('',#3724,#3714,#2442,.T.);
#4794=EDGE_CURVE('',#3716,#3725,#2443,.T.);
#4795=EDGE_CURVE('',#3726,#3726,#1505,.T.);
#4796=EDGE_CURVE('',#3727,#3727,#1506,.T.);
#4797=EDGE_CURVE('',#3726,#3728,#2444,.T.);
#4798=EDGE_CURVE('',#3728,#3728,#1507,.T.);
#4799=EDGE_CURVE('',#3711,#3727,#2445,.T.);
#4800=EDGE_CURVE('',#3729,#3730,#2446,.T.);
#4801=EDGE_CURVE('',#3729,#3731,#2447,.T.);
#4802=EDGE_CURVE('',#3732,#3731,#2448,.T.);
#4803=EDGE_CURVE('',#3730,#3732,#2449,.T.);
#4804=EDGE_CURVE('',#3733,#3729,#2450,.T.);
#4805=EDGE_CURVE('',#3733,#3734,#2451,.T.);
#4806=EDGE_CURVE('',#3731,#3734,#2452,.T.);
#4807=EDGE_CURVE('',#3735,#3733,#2453,.T.);
#4808=EDGE_CURVE('',#3735,#3736,#2454,.T.);
#4809=EDGE_CURVE('',#3734,#3736,#2455,.T.);
#4810=EDGE_CURVE('',#3737,#3735,#2456,.T.);
#4811=EDGE_CURVE('',#3737,#3738,#2457,.T.);
#4812=EDGE_CURVE('',#3736,#3738,#2458,.T.);
#4813=EDGE_CURVE('',#3739,#3737,#2459,.T.);
#4814=EDGE_CURVE('',#3739,#3740,#2460,.T.);
#4815=EDGE_CURVE('',#3738,#3740,#2461,.T.);
#4816=EDGE_CURVE('',#3730,#3739,#2462,.T.);
#4817=EDGE_CURVE('',#3740,#3732,#2463,.T.);
#4818=EDGE_CURVE('',#3741,#3742,#2464,.T.);
#4819=EDGE_CURVE('',#3742,#3743,#2465,.T.);
#4820=EDGE_CURVE('',#3744,#3743,#2466,.T.);
#4821=EDGE_CURVE('',#3741,#3744,#2467,.T.);
#4822=EDGE_CURVE('',#3745,#3741,#2468,.T.);
#4823=EDGE_CURVE('',#3746,#3744,#2469,.T.);
#4824=EDGE_CURVE('',#3745,#3746,#2470,.T.);
#4825=EDGE_CURVE('',#3747,#3745,#2471,.T.);
#4826=EDGE_CURVE('',#3748,#3746,#2472,.T.);
#4827=EDGE_CURVE('',#3747,#3748,#2473,.T.);
#4828=EDGE_CURVE('',#3742,#3747,#2474,.T.);
#4829=EDGE_CURVE('',#3743,#3748,#2475,.T.);
#4830=EDGE_CURVE('',#3749,#3749,#1508,.T.);
#4831=EDGE_CURVE('',#3749,#3750,#2476,.T.);
#4832=EDGE_CURVE('',#3750,#3750,#1509,.T.);
#4833=EDGE_CURVE('',#3751,#3751,#1510,.T.);
#4834=EDGE_CURVE('',#3751,#3752,#2477,.T.);
#4835=EDGE_CURVE('',#3752,#3752,#1511,.T.);
#4836=EDGE_CURVE('',#3753,#3754,#2478,.T.);
#4837=EDGE_CURVE('',#3755,#3753,#2479,.T.);
#4838=EDGE_CURVE('',#3756,#3755,#2480,.T.);
#4839=EDGE_CURVE('',#3754,#3756,#2481,.T.);
#4840=EDGE_CURVE('',#3757,#3758,#2482,.T.);
#4841=EDGE_CURVE('',#3759,#3757,#2483,.T.);
#4842=EDGE_CURVE('',#3760,#3759,#2484,.T.);
#4843=EDGE_CURVE('',#3758,#3760,#2485,.T.);
#4844=EDGE_CURVE('',#3755,#3760,#1512,.T.);
#4845=EDGE_CURVE('',#3758,#3753,#1513,.T.);
#4846=EDGE_CURVE('',#3757,#3754,#1514,.T.);
#4847=EDGE_CURVE('',#3756,#3759,#1515,.T.);
#4848=EDGE_CURVE('',#3761,#3761,#1516,.T.);
#4849=EDGE_CURVE('',#3761,#3762,#2486,.T.);
#4850=EDGE_CURVE('',#3762,#3762,#1517,.T.);
#4851=EDGE_CURVE('',#3763,#3763,#1518,.T.);
#4852=EDGE_CURVE('',#3763,#3764,#2487,.T.);
#4853=EDGE_CURVE('',#3764,#3764,#1519,.T.);
#4854=EDGE_CURVE('',#3765,#3766,#2488,.T.);
#4855=EDGE_CURVE('',#3765,#3767,#1960,.T.);
#4856=EDGE_CURVE('',#3767,#3768,#1520,.F.);
#4857=EDGE_CURVE('',#3768,#3766,#1961,.T.);
#4858=EDGE_CURVE('',#3769,#3770,#2489,.T.);
#4859=EDGE_CURVE('',#3769,#3765,#1962,.T.);
#4860=EDGE_CURVE('',#3766,#3770,#1963,.T.);
#4861=EDGE_CURVE('',#3771,#3772,#2490,.T.);
#4862=EDGE_CURVE('',#3771,#3769,#1964,.T.);
#4863=EDGE_CURVE('',#3770,#3772,#1965,.T.);
#4864=EDGE_CURVE('',#3773,#3774,#2491,.T.);
#4865=EDGE_CURVE('',#3773,#3771,#1966,.T.);
#4866=EDGE_CURVE('',#3772,#3774,#1967,.T.);
#4867=EDGE_CURVE('',#3775,#3776,#2492,.T.);
#4868=EDGE_CURVE('',#3775,#3773,#1968,.T.);
#4869=EDGE_CURVE('',#3774,#3776,#1969,.T.);
#4870=EDGE_CURVE('',#3777,#3778,#2493,.T.);
#4871=EDGE_CURVE('',#3777,#3775,#1970,.T.);
#4872=EDGE_CURVE('',#3776,#3778,#1971,.T.);
#4873=EDGE_CURVE('',#3779,#3780,#2494,.T.);
#4874=EDGE_CURVE('',#3779,#3777,#1972,.T.);
#4875=EDGE_CURVE('',#3778,#3780,#1973,.T.);
#4876=EDGE_CURVE('',#3781,#3782,#2495,.T.);
#4877=EDGE_CURVE('',#3781,#3779,#1974,.T.);
#4878=EDGE_CURVE('',#3780,#3782,#1975,.T.);
#4879=EDGE_CURVE('',#3783,#3784,#2496,.T.);
#4880=EDGE_CURVE('',#3783,#3781,#1976,.T.);
#4881=EDGE_CURVE('',#3782,#3784,#1977,.T.);
#4882=EDGE_CURVE('',#3785,#3786,#2497,.T.);
#4883=EDGE_CURVE('',#3785,#3783,#1978,.T.);
#4884=EDGE_CURVE('',#3784,#3786,#1979,.T.);
#4885=EDGE_CURVE('',#3787,#3788,#2498,.T.);
#4886=EDGE_CURVE('',#3787,#3789,#1980,.T.);
#4887=EDGE_CURVE('',#3789,#3790,#1521,.T.);
#4888=EDGE_CURVE('',#3788,#3790,#1981,.T.);
#4889=EDGE_CURVE('',#3791,#3792,#2499,.T.);
#4890=EDGE_CURVE('',#3791,#3787,#1982,.T.);
#4891=EDGE_CURVE('',#3792,#3788,#1983,.T.);
#4892=EDGE_CURVE('',#3793,#3794,#2500,.T.);
#4893=EDGE_CURVE('',#3793,#3791,#1984,.T.);
#4894=EDGE_CURVE('',#3794,#3792,#1985,.T.);
#4895=EDGE_CURVE('',#3795,#3796,#2501,.T.);
#4896=EDGE_CURVE('',#3795,#3793,#1986,.T.);
#4897=EDGE_CURVE('',#3796,#3794,#1987,.T.);
#4898=EDGE_CURVE('',#3797,#3798,#2502,.T.);
#4899=EDGE_CURVE('',#3797,#3795,#1988,.T.);
#4900=EDGE_CURVE('',#3798,#3796,#1989,.T.);
#4901=EDGE_CURVE('',#3799,#3800,#2503,.T.);
#4902=EDGE_CURVE('',#3799,#3797,#1990,.T.);
#4903=EDGE_CURVE('',#3800,#3798,#1991,.T.);
#4904=EDGE_CURVE('',#3801,#3802,#2504,.T.);
#4905=EDGE_CURVE('',#3801,#3799,#1992,.T.);
#4906=EDGE_CURVE('',#3802,#3800,#1993,.T.);
#4907=EDGE_CURVE('',#3803,#3804,#2505,.T.);
#4908=EDGE_CURVE('',#3803,#3801,#1994,.T.);
#4909=EDGE_CURVE('',#3804,#3802,#1995,.T.);
#4910=EDGE_CURVE('',#3805,#3806,#2506,.T.);
#4911=EDGE_CURVE('',#3805,#3803,#1996,.T.);
#4912=EDGE_CURVE('',#3806,#3804,#1997,.T.);
#4913=EDGE_CURVE('',#3807,#3808,#2507,.T.);
#4914=EDGE_CURVE('',#3807,#3805,#1998,.T.);
#4915=EDGE_CURVE('',#3808,#3806,#1999,.T.);
#4916=EDGE_CURVE('',#3790,#3809,#2000,.T.);
#4917=EDGE_CURVE('',#3810,#3789,#2001,.T.);
#4918=EDGE_CURVE('',#3811,#3810,#1522,.T.);
#4919=EDGE_CURVE('',#3809,#3811,#2002,.T.);
#4920=EDGE_CURVE('',#3809,#3812,#2508,.T.);
#4921=EDGE_CURVE('',#3812,#3812,#1523,.T.);
#4922=EDGE_CURVE('',#3813,#3807,#2003,.T.);
#4923=EDGE_CURVE('',#3767,#3813,#2004,.T.);
#4924=EDGE_CURVE('',#3810,#3785,#2005,.T.);
#4925=EDGE_CURVE('',#3814,#3808,#2006,.T.);
#4926=EDGE_CURVE('',#3813,#3814,#1524,.T.);
#4927=EDGE_CURVE('',#3786,#3811,#2007,.T.);
#4928=EDGE_CURVE('',#3814,#3768,#2008,.T.);
#4929=EDGE_CURVE('',#3815,#3816,#2509,.T.);
#4930=EDGE_CURVE('',#3815,#3817,#2510,.T.);
#4931=EDGE_CURVE('',#3817,#3818,#2511,.T.);
#4932=EDGE_CURVE('',#3816,#3818,#2512,.T.);
#4933=EDGE_CURVE('',#3819,#3815,#2513,.T.);
#4934=EDGE_CURVE('',#3819,#3820,#2514,.T.);
#4935=EDGE_CURVE('',#3820,#3817,#2515,.T.);
#4936=EDGE_CURVE('',#3821,#3819,#2516,.T.);
#4937=EDGE_CURVE('',#3821,#3822,#2517,.T.);
#4938=EDGE_CURVE('',#3822,#3820,#2518,.T.);
#4939=EDGE_CURVE('',#3823,#3821,#2519,.T.);
#4940=EDGE_CURVE('',#3823,#3824,#2520,.T.);
#4941=EDGE_CURVE('',#3824,#3822,#2521,.T.);
#4942=EDGE_CURVE('',#3825,#3823,#2522,.T.);
#4943=EDGE_CURVE('',#3825,#3826,#2523,.T.);
#4944=EDGE_CURVE('',#3826,#3824,#2524,.T.);
#4945=EDGE_CURVE('',#3816,#3825,#2525,.T.);
#4946=EDGE_CURVE('',#3818,#3826,#2526,.T.);
#4947=EDGE_CURVE('',#3827,#3827,#1525,.T.);
#4948=EDGE_CURVE('',#3827,#3828,#2527,.T.);
#4949=EDGE_CURVE('',#3828,#3828,#1526,.T.);
#4950=EDGE_CURVE('',#3829,#3830,#2528,.T.);
#4951=EDGE_CURVE('',#3829,#3831,#2529,.T.);
#4952=EDGE_CURVE('',#3832,#3831,#2530,.T.);
#4953=EDGE_CURVE('',#3830,#3832,#2531,.T.);
#4954=EDGE_CURVE('',#3833,#3829,#2532,.T.);
#4955=EDGE_CURVE('',#3830,#3834,#2533,.T.);
#4956=EDGE_CURVE('',#3834,#3835,#2534,.T.);
#4957=EDGE_CURVE('',#3835,#3836,#2535,.T.);
#4958=EDGE_CURVE('',#3836,#3837,#2536,.T.);
#4959=EDGE_CURVE('',#3837,#3838,#2537,.T.);
#4960=EDGE_CURVE('',#3838,#3833,#2538,.T.);
#4961=EDGE_CURVE('',#3839,#3839,#1527,.T.);
#4962=EDGE_CURVE('',#3840,#3840,#1528,.T.);
#4963=EDGE_CURVE('',#3840,#3841,#2539,.T.);
#4964=EDGE_CURVE('',#3841,#3841,#1529,.T.);
#4965=EDGE_CURVE('',#3839,#3842,#2540,.T.);
#4966=EDGE_CURVE('',#3842,#3842,#1530,.T.);
#4967=EDGE_CURVE('',#3843,#3844,#2541,.T.);
#4968=EDGE_CURVE('',#3835,#3843,#1531,.T.);
#4969=EDGE_CURVE('',#3834,#3844,#1532,.T.);
#4970=EDGE_CURVE('',#3845,#3845,#1533,.T.);
#4971=EDGE_CURVE('',#3845,#3846,#2542,.T.);
#4972=EDGE_CURVE('',#3846,#3846,#1534,.T.);
#4973=EDGE_CURVE('',#3844,#3832,#2543,.T.);
#4974=EDGE_CURVE('',#3831,#3847,#2544,.T.);
#4975=EDGE_CURVE('',#3833,#3847,#1535,.T.);
#4976=EDGE_CURVE('',#3848,#3848,#1536,.T.);
#4977=EDGE_CURVE('',#3848,#3849,#2545,.T.);
#4978=EDGE_CURVE('',#3849,#3849,#1537,.T.);
#4979=EDGE_CURVE('',#3847,#3850,#2546,.T.);
#4980=EDGE_CURVE('',#3838,#3850,#1538,.T.);
#4981=EDGE_CURVE('',#3851,#3837,#2547,.T.);
#4982=EDGE_CURVE('',#3851,#3850,#2548,.T.);
#4983=EDGE_CURVE('',#3843,#3852,#2549,.T.);
#4984=EDGE_CURVE('',#3852,#3836,#2550,.T.);
#4985=EDGE_CURVE('',#3852,#3851,#2551,.T.);
#4986=EDGE_CURVE('',#3853,#3853,#1539,.T.);
#4987=EDGE_CURVE('',#3853,#3854,#2552,.T.);
#4988=EDGE_CURVE('',#3854,#3854,#1540,.T.);
#4989=EDGE_CURVE('',#3855,#3855,#1541,.T.);
#4990=EDGE_CURVE('',#3856,#3856,#1542,.T.);
#4991=EDGE_CURVE('',#3857,#3857,#1543,.T.);
#4992=EDGE_CURVE('',#3857,#3856,#2553,.T.);
#4993=EDGE_CURVE('',#3858,#3858,#1544,.T.);
#4994=EDGE_CURVE('',#3859,#3859,#1545,.T.);
#4995=EDGE_CURVE('',#3858,#3860,#2554,.T.);
#4996=EDGE_CURVE('',#3860,#3860,#1546,.T.);
#4997=EDGE_CURVE('',#3855,#3859,#2555,.T.);
#4998=EDGE_CURVE('',#3861,#3862,#2556,.T.);
#4999=EDGE_CURVE('',#3863,#3861,#2557,.T.);
#5000=EDGE_CURVE('',#3864,#3863,#2558,.T.);
#5001=EDGE_CURVE('',#3862,#3864,#2559,.T.);
#5002=EDGE_CURVE('',#3865,#3866,#2560,.T.);
#5003=EDGE_CURVE('',#3867,#3865,#2561,.T.);
#5004=EDGE_CURVE('',#3868,#3867,#2562,.T.);
#5005=EDGE_CURVE('',#3866,#3868,#2563,.T.);
#5006=EDGE_CURVE('',#3863,#3868,#1547,.T.);
#5007=EDGE_CURVE('',#3866,#3861,#1548,.T.);
#5008=EDGE_CURVE('',#3865,#3862,#1549,.T.);
#5009=EDGE_CURVE('',#3864,#3867,#1550,.T.);
#5010=EDGE_CURVE('',#3869,#3870,#2564,.T.);
#5011=EDGE_CURVE('',#3869,#3871,#2565,.T.);
#5012=EDGE_CURVE('',#3872,#3871,#2566,.T.);
#5013=EDGE_CURVE('',#3870,#3872,#2567,.T.);
#5014=EDGE_CURVE('',#3873,#3874,#2568,.T.);
#5015=EDGE_CURVE('',#3875,#3873,#2569,.T.);
#5016=EDGE_CURVE('',#3876,#3875,#2570,.T.);
#5017=EDGE_CURVE('',#3874,#3876,#2571,.T.);
#5018=EDGE_CURVE('',#3871,#3877,#2572,.T.);
#5019=EDGE_CURVE('',#3877,#3878,#2573,.T.);
#5020=EDGE_CURVE('',#3878,#3876,#2574,.T.);
#5021=EDGE_CURVE('',#3879,#3875,#2575,.T.);
#5022=EDGE_CURVE('',#3880,#3879,#2576,.T.);
#5023=EDGE_CURVE('',#3872,#3880,#2577,.T.);
#5024=EDGE_CURVE('',#3881,#3881,#1551,.T.);
#5025=EDGE_CURVE('',#3882,#3882,#1552,.T.);
#5026=EDGE_CURVE('',#3883,#3873,#2578,.T.);
#5027=EDGE_CURVE('',#3879,#3883,#2579,.T.);
#5028=EDGE_CURVE('',#3884,#3884,#1553,.T.);
#5029=EDGE_CURVE('',#3884,#3882,#2580,.T.);
#5030=EDGE_CURVE('',#3885,#3885,#1554,.T.);
#5031=EDGE_CURVE('',#3885,#3881,#2581,.T.);
#5032=EDGE_CURVE('',#3878,#3886,#1555,.T.);
#5033=EDGE_CURVE('',#3874,#3886,#2582,.T.);
#5034=EDGE_CURVE('',#3887,#3887,#1556,.T.);
#5035=EDGE_CURVE('',#3887,#3888,#2583,.T.);
#5036=EDGE_CURVE('',#3888,#3888,#1557,.T.);
#5037=EDGE_CURVE('',#3886,#3889,#2584,.T.);
#5038=EDGE_CURVE('',#3877,#3889,#1558,.T.);
#5039=EDGE_CURVE('',#3889,#3869,#2585,.T.);
#5040=EDGE_CURVE('',#3890,#3883,#2586,.T.);
#5041=EDGE_CURVE('',#3880,#3890,#2587,.T.);
#5042=EDGE_CURVE('',#3870,#3890,#2588,.T.);
#5043=EDGE_CURVE('',#3891,#3891,#1559,.T.);
#5044=EDGE_CURVE('',#3891,#3892,#2589,.T.);
#5045=EDGE_CURVE('',#3892,#3892,#1560,.T.);
#5046=EDGE_CURVE('',#3893,#3893,#1561,.T.);
#5047=EDGE_CURVE('',#3893,#3894,#2590,.T.);
#5048=EDGE_CURVE('',#3894,#3894,#1562,.T.);
#5049=EDGE_CURVE('',#3895,#3896,#2591,.T.);
#5050=EDGE_CURVE('',#3895,#3897,#2009,.T.);
#5051=EDGE_CURVE('',#3897,#3898,#1563,.F.);
#5052=EDGE_CURVE('',#3898,#3896,#2010,.T.);
#5053=EDGE_CURVE('',#3899,#3900,#2592,.T.);
#5054=EDGE_CURVE('',#3899,#3895,#2011,.T.);
#5055=EDGE_CURVE('',#3896,#3900,#2012,.T.);
#5056=EDGE_CURVE('',#3901,#3902,#2593,.T.);
#5057=EDGE_CURVE('',#3901,#3899,#2013,.T.);
#5058=EDGE_CURVE('',#3900,#3902,#2014,.T.);
#5059=EDGE_CURVE('',#3903,#3904,#2594,.T.);
#5060=EDGE_CURVE('',#3903,#3901,#2015,.T.);
#5061=EDGE_CURVE('',#3902,#3904,#2016,.T.);
#5062=EDGE_CURVE('',#3905,#3906,#2595,.T.);
#5063=EDGE_CURVE('',#3905,#3903,#2017,.T.);
#5064=EDGE_CURVE('',#3904,#3906,#2018,.T.);
#5065=EDGE_CURVE('',#3907,#3908,#2596,.T.);
#5066=EDGE_CURVE('',#3907,#3905,#2019,.T.);
#5067=EDGE_CURVE('',#3906,#3908,#2020,.T.);
#5068=EDGE_CURVE('',#3909,#3910,#2597,.T.);
#5069=EDGE_CURVE('',#3909,#3907,#2021,.T.);
#5070=EDGE_CURVE('',#3908,#3910,#2022,.T.);
#5071=EDGE_CURVE('',#3911,#3912,#2598,.T.);
#5072=EDGE_CURVE('',#3911,#3909,#2023,.T.);
#5073=EDGE_CURVE('',#3910,#3912,#2024,.T.);
#5074=EDGE_CURVE('',#3913,#3914,#2599,.T.);
#5075=EDGE_CURVE('',#3913,#3911,#2025,.T.);
#5076=EDGE_CURVE('',#3912,#3914,#2026,.T.);
#5077=EDGE_CURVE('',#3915,#3916,#2600,.T.);
#5078=EDGE_CURVE('',#3915,#3913,#2027,.T.);
#5079=EDGE_CURVE('',#3914,#3916,#2028,.T.);
#5080=EDGE_CURVE('',#3917,#3918,#2601,.T.);
#5081=EDGE_CURVE('',#3917,#3915,#2029,.T.);
#5082=EDGE_CURVE('',#3916,#3918,#2030,.T.);
#5083=EDGE_CURVE('',#3919,#3920,#2602,.T.);
#5084=EDGE_CURVE('',#3919,#3917,#2031,.T.);
#5085=EDGE_CURVE('',#3918,#3920,#2032,.T.);
#5086=EDGE_CURVE('',#3921,#3922,#2603,.T.);
#5087=EDGE_CURVE('',#3921,#3919,#2033,.T.);
#5088=EDGE_CURVE('',#3920,#3922,#2034,.T.);
#5089=EDGE_CURVE('',#3923,#3924,#2604,.T.);
#5090=EDGE_CURVE('',#3923,#3921,#2035,.T.);
#5091=EDGE_CURVE('',#3922,#3924,#2036,.T.);
#5092=EDGE_CURVE('',#3925,#3926,#2605,.T.);
#5093=EDGE_CURVE('',#3925,#3923,#2037,.T.);
#5094=EDGE_CURVE('',#3924,#3926,#2038,.T.);
#5095=EDGE_CURVE('',#3927,#3928,#2606,.T.);
#5096=EDGE_CURVE('',#3927,#3925,#2039,.T.);
#5097=EDGE_CURVE('',#3926,#3928,#2040,.T.);
#5098=EDGE_CURVE('',#3929,#3930,#2607,.T.);
#5099=EDGE_CURVE('',#3929,#3927,#2041,.T.);
#5100=EDGE_CURVE('',#3928,#3930,#2042,.T.);
#5101=EDGE_CURVE('',#3931,#3932,#2608,.T.);
#5102=EDGE_CURVE('',#3931,#3929,#2043,.T.);
#5103=EDGE_CURVE('',#3930,#3932,#2044,.T.);
#5104=EDGE_CURVE('',#3933,#3934,#2609,.T.);
#5105=EDGE_CURVE('',#3933,#3931,#2045,.T.);
#5106=EDGE_CURVE('',#3932,#3934,#2046,.T.);
#5107=EDGE_CURVE('',#3935,#3936,#2610,.T.);
#5108=EDGE_CURVE('',#3935,#3937,#2047,.T.);
#5109=EDGE_CURVE('',#3937,#3938,#1564,.T.);
#5110=EDGE_CURVE('',#3936,#3938,#2048,.T.);
#5111=EDGE_CURVE('',#3939,#3940,#2611,.T.);
#5112=EDGE_CURVE('',#3939,#3935,#2049,.T.);
#5113=EDGE_CURVE('',#3940,#3936,#2050,.T.);
#5114=EDGE_CURVE('',#3941,#3942,#2612,.T.);
#5115=EDGE_CURVE('',#3941,#3939,#2051,.T.);
#5116=EDGE_CURVE('',#3942,#3940,#2052,.T.);
#5117=EDGE_CURVE('',#3943,#3944,#2613,.T.);
#5118=EDGE_CURVE('',#3943,#3941,#2053,.T.);
#5119=EDGE_CURVE('',#3944,#3942,#2054,.T.);
#5120=EDGE_CURVE('',#3945,#3946,#2614,.T.);
#5121=EDGE_CURVE('',#3945,#3943,#2055,.T.);
#5122=EDGE_CURVE('',#3946,#3944,#2056,.T.);
#5123=EDGE_CURVE('',#3947,#3948,#2615,.T.);
#5124=EDGE_CURVE('',#3947,#3945,#2057,.T.);
#5125=EDGE_CURVE('',#3948,#3946,#2058,.T.);
#5126=EDGE_CURVE('',#3949,#3950,#2616,.T.);
#5127=EDGE_CURVE('',#3949,#3947,#2059,.T.);
#5128=EDGE_CURVE('',#3950,#3948,#2060,.T.);
#5129=EDGE_CURVE('',#3951,#3952,#2617,.T.);
#5130=EDGE_CURVE('',#3951,#3949,#2061,.T.);
#5131=EDGE_CURVE('',#3952,#3950,#2062,.T.);
#5132=EDGE_CURVE('',#3953,#3954,#2618,.T.);
#5133=EDGE_CURVE('',#3953,#3951,#2063,.T.);
#5134=EDGE_CURVE('',#3954,#3952,#2064,.T.);
#5135=EDGE_CURVE('',#3955,#3956,#2619,.T.);
#5136=EDGE_CURVE('',#3955,#3953,#2065,.T.);
#5137=EDGE_CURVE('',#3956,#3954,#2066,.T.);
#5138=EDGE_CURVE('',#3957,#3958,#2620,.T.);
#5139=EDGE_CURVE('',#3957,#3955,#2067,.T.);
#5140=EDGE_CURVE('',#3958,#3956,#2068,.T.);
#5141=EDGE_CURVE('',#3959,#3960,#2621,.T.);
#5142=EDGE_CURVE('',#3959,#3957,#2069,.T.);
#5143=EDGE_CURVE('',#3960,#3958,#2070,.T.);
#5144=EDGE_CURVE('',#3961,#3962,#2622,.T.);
#5145=EDGE_CURVE('',#3961,#3959,#2071,.T.);
#5146=EDGE_CURVE('',#3962,#3960,#2072,.T.);
#5147=EDGE_CURVE('',#3963,#3964,#2623,.T.);
#5148=EDGE_CURVE('',#3963,#3961,#2073,.T.);
#5149=EDGE_CURVE('',#3964,#3962,#2074,.T.);
#5150=EDGE_CURVE('',#3965,#3966,#2624,.T.);
#5151=EDGE_CURVE('',#3965,#3963,#2075,.T.);
#5152=EDGE_CURVE('',#3966,#3964,#2076,.T.);
#5153=EDGE_CURVE('',#3967,#3968,#2625,.T.);
#5154=EDGE_CURVE('',#3967,#3965,#2077,.T.);
#5155=EDGE_CURVE('',#3968,#3966,#2078,.T.);
#5156=EDGE_CURVE('',#3969,#3970,#2626,.T.);
#5157=EDGE_CURVE('',#3969,#3967,#2079,.T.);
#5158=EDGE_CURVE('',#3970,#3968,#2080,.T.);
#5159=EDGE_CURVE('',#3971,#3972,#2627,.T.);
#5160=EDGE_CURVE('',#3971,#3969,#2081,.T.);
#5161=EDGE_CURVE('',#3972,#3970,#2082,.T.);
#5162=EDGE_CURVE('',#3973,#3974,#2628,.T.);
#5163=EDGE_CURVE('',#3973,#3971,#2083,.T.);
#5164=EDGE_CURVE('',#3974,#3972,#2084,.T.);
#5165=EDGE_CURVE('',#3938,#3975,#2085,.T.);
#5166=EDGE_CURVE('',#3976,#3937,#2086,.T.);
#5167=EDGE_CURVE('',#3977,#3976,#1565,.T.);
#5168=EDGE_CURVE('',#3975,#3977,#2087,.T.);
#5169=EDGE_CURVE('',#3975,#3978,#2629,.T.);
#5170=EDGE_CURVE('',#3978,#3978,#1566,.T.);
#5171=EDGE_CURVE('',#3979,#3973,#2088,.T.);
#5172=EDGE_CURVE('',#3897,#3979,#2089,.T.);
#5173=EDGE_CURVE('',#3976,#3933,#2090,.T.);
#5174=EDGE_CURVE('',#3980,#3974,#2091,.T.);
#5175=EDGE_CURVE('',#3979,#3980,#1567,.T.);
#5176=EDGE_CURVE('',#3934,#3977,#2092,.T.);
#5177=EDGE_CURVE('',#3980,#3898,#2093,.T.);
#5178=EDGE_CURVE('',#3981,#3982,#2630,.T.);
#5179=EDGE_CURVE('',#3981,#3983,#2631,.T.);
#5180=EDGE_CURVE('',#3983,#3984,#2632,.T.);
#5181=EDGE_CURVE('',#3982,#3984,#2633,.T.);
#5182=EDGE_CURVE('',#3985,#3981,#2634,.T.);
#5183=EDGE_CURVE('',#3985,#3986,#2635,.T.);
#5184=EDGE_CURVE('',#3986,#3983,#2636,.T.);
#5185=EDGE_CURVE('',#3987,#3985,#2637,.T.);
#5186=EDGE_CURVE('',#3987,#3988,#2638,.T.);
#5187=EDGE_CURVE('',#3988,#3986,#2639,.T.);
#5188=EDGE_CURVE('',#3989,#3987,#2640,.T.);
#5189=EDGE_CURVE('',#3989,#3990,#2641,.T.);
#5190=EDGE_CURVE('',#3990,#3988,#2642,.T.);
#5191=EDGE_CURVE('',#3991,#3989,#2643,.T.);
#5192=EDGE_CURVE('',#3991,#3992,#2644,.T.);
#5193=EDGE_CURVE('',#3992,#3990,#2645,.T.);
#5194=EDGE_CURVE('',#3982,#3991,#2646,.T.);
#5195=EDGE_CURVE('',#3984,#3992,#2647,.T.);
#5196=EDGE_CURVE('',#3993,#3993,#1568,.T.);
#5197=EDGE_CURVE('',#3993,#3994,#2648,.T.);
#5198=EDGE_CURVE('',#3994,#3994,#1569,.T.);
#5199=EDGE_CURVE('',#3995,#3996,#2649,.T.);
#5200=EDGE_CURVE('',#3995,#3997,#2094,.T.);
#5201=EDGE_CURVE('',#3997,#3998,#1570,.F.);
#5202=EDGE_CURVE('',#3998,#3996,#2095,.T.);
#5203=EDGE_CURVE('',#3999,#4000,#2650,.T.);
#5204=EDGE_CURVE('',#3999,#3995,#2096,.T.);
#5205=EDGE_CURVE('',#3996,#4000,#2097,.T.);
#5206=EDGE_CURVE('',#4001,#4002,#2651,.T.);
#5207=EDGE_CURVE('',#4001,#3999,#2098,.T.);
#5208=EDGE_CURVE('',#4000,#4002,#2099,.T.);
#5209=EDGE_CURVE('',#4003,#4004,#2652,.T.);
#5210=EDGE_CURVE('',#4003,#4001,#2100,.T.);
#5211=EDGE_CURVE('',#4002,#4004,#2101,.T.);
#5212=EDGE_CURVE('',#4005,#4006,#2653,.T.);
#5213=EDGE_CURVE('',#4005,#4003,#2102,.T.);
#5214=EDGE_CURVE('',#4004,#4006,#2103,.T.);
#5215=EDGE_CURVE('',#4007,#4008,#2654,.T.);
#5216=EDGE_CURVE('',#4007,#4005,#2104,.T.);
#5217=EDGE_CURVE('',#4006,#4008,#2105,.T.);
#5218=EDGE_CURVE('',#4009,#4010,#2655,.T.);
#5219=EDGE_CURVE('',#4009,#4007,#2106,.T.);
#5220=EDGE_CURVE('',#4008,#4010,#2107,.T.);
#5221=EDGE_CURVE('',#4011,#4012,#2656,.T.);
#5222=EDGE_CURVE('',#4011,#4009,#2108,.T.);
#5223=EDGE_CURVE('',#4010,#4012,#2109,.T.);
#5224=EDGE_CURVE('',#4013,#4014,#2657,.T.);
#5225=EDGE_CURVE('',#4013,#4011,#2110,.T.);
#5226=EDGE_CURVE('',#4012,#4014,#2111,.T.);
#5227=EDGE_CURVE('',#4015,#4016,#2658,.T.);
#5228=EDGE_CURVE('',#4015,#4013,#2112,.T.);
#5229=EDGE_CURVE('',#4014,#4016,#2113,.T.);
#5230=EDGE_CURVE('',#4017,#4018,#2659,.T.);
#5231=EDGE_CURVE('',#4017,#4015,#2114,.T.);
#5232=EDGE_CURVE('',#4016,#4018,#2115,.T.);
#5233=EDGE_CURVE('',#4019,#4020,#2660,.T.);
#5234=EDGE_CURVE('',#4019,#4021,#2116,.T.);
#5235=EDGE_CURVE('',#4021,#4022,#1571,.T.);
#5236=EDGE_CURVE('',#4020,#4022,#2117,.T.);
#5237=EDGE_CURVE('',#4023,#4024,#2661,.T.);
#5238=EDGE_CURVE('',#4023,#4019,#2118,.T.);
#5239=EDGE_CURVE('',#4024,#4020,#2119,.T.);
#5240=EDGE_CURVE('',#4025,#4026,#2662,.T.);
#5241=EDGE_CURVE('',#4025,#4023,#2120,.T.);
#5242=EDGE_CURVE('',#4026,#4024,#2121,.T.);
#5243=EDGE_CURVE('',#4027,#4028,#2663,.T.);
#5244=EDGE_CURVE('',#4027,#4025,#2122,.T.);
#5245=EDGE_CURVE('',#4028,#4026,#2123,.T.);
#5246=EDGE_CURVE('',#4029,#4030,#2664,.T.);
#5247=EDGE_CURVE('',#4029,#4027,#2124,.T.);
#5248=EDGE_CURVE('',#4030,#4028,#2125,.T.);
#5249=EDGE_CURVE('',#4031,#4032,#2665,.T.);
#5250=EDGE_CURVE('',#4031,#4029,#2126,.T.);
#5251=EDGE_CURVE('',#4032,#4030,#2127,.T.);
#5252=EDGE_CURVE('',#4033,#4034,#2666,.T.);
#5253=EDGE_CURVE('',#4033,#4031,#2128,.T.);
#5254=EDGE_CURVE('',#4034,#4032,#2129,.T.);
#5255=EDGE_CURVE('',#4035,#4036,#2667,.T.);
#5256=EDGE_CURVE('',#4035,#4033,#2130,.T.);
#5257=EDGE_CURVE('',#4036,#4034,#2131,.T.);
#5258=EDGE_CURVE('',#4037,#4038,#2668,.T.);
#5259=EDGE_CURVE('',#4037,#4035,#2132,.T.);
#5260=EDGE_CURVE('',#4038,#4036,#2133,.T.);
#5261=EDGE_CURVE('',#4039,#4040,#2669,.T.);
#5262=EDGE_CURVE('',#4039,#4037,#2134,.T.);
#5263=EDGE_CURVE('',#4040,#4038,#2135,.T.);
#5264=EDGE_CURVE('',#4041,#4042,#2670,.T.);
#5265=EDGE_CURVE('',#4041,#4039,#2136,.T.);
#5266=EDGE_CURVE('',#4042,#4040,#2137,.T.);
#5267=EDGE_CURVE('',#4022,#4043,#2138,.T.);
#5268=EDGE_CURVE('',#4044,#4021,#2139,.T.);
#5269=EDGE_CURVE('',#4045,#4044,#1572,.T.);
#5270=EDGE_CURVE('',#4043,#4045,#2140,.T.);
#5271=EDGE_CURVE('',#4043,#4046,#2671,.T.);
#5272=EDGE_CURVE('',#4046,#4046,#1573,.T.);
#5273=EDGE_CURVE('',#4047,#4041,#2141,.T.);
#5274=EDGE_CURVE('',#3997,#4047,#2142,.T.);
#5275=EDGE_CURVE('',#4044,#4017,#2143,.T.);
#5276=EDGE_CURVE('',#4048,#4042,#2144,.T.);
#5277=EDGE_CURVE('',#4047,#4048,#1574,.T.);
#5278=EDGE_CURVE('',#4018,#4045,#2145,.T.);
#5279=EDGE_CURVE('',#4048,#3998,#2146,.T.);
#5280=EDGE_CURVE('',#4049,#4050,#2672,.T.);
#5281=EDGE_CURVE('',#4049,#4051,#2673,.T.);
#5282=EDGE_CURVE('',#4051,#4052,#2674,.T.);
#5283=EDGE_CURVE('',#4050,#4052,#2675,.T.);
#5284=EDGE_CURVE('',#4053,#4049,#2676,.T.);
#5285=EDGE_CURVE('',#4053,#4054,#2677,.T.);
#5286=EDGE_CURVE('',#4054,#4051,#2678,.T.);
#5287=EDGE_CURVE('',#4055,#4053,#2679,.T.);
#5288=EDGE_CURVE('',#4055,#4056,#2680,.T.);
#5289=EDGE_CURVE('',#4056,#4054,#2681,.T.);
#5290=EDGE_CURVE('',#4057,#4055,#2682,.T.);
#5291=EDGE_CURVE('',#4057,#4058,#2683,.T.);
#5292=EDGE_CURVE('',#4058,#4056,#2684,.T.);
#5293=EDGE_CURVE('',#4059,#4057,#2685,.T.);
#5294=EDGE_CURVE('',#4059,#4060,#2686,.T.);
#5295=EDGE_CURVE('',#4060,#4058,#2687,.T.);
#5296=EDGE_CURVE('',#4050,#4059,#2688,.T.);
#5297=EDGE_CURVE('',#4052,#4060,#2689,.T.);
#5298=EDGE_CURVE('',#4061,#4061,#1575,.T.);
#5299=EDGE_CURVE('',#4061,#4062,#2690,.T.);
#5300=EDGE_CURVE('',#4062,#4062,#1576,.T.);
#5301=EDGE_CURVE('',#4063,#4063,#1577,.T.);
#5302=EDGE_CURVE('',#4063,#4064,#2691,.T.);
#5303=EDGE_CURVE('',#4064,#4064,#1578,.T.);
#5304=EDGE_CURVE('',#4065,#4065,#1579,.T.);
#5305=EDGE_CURVE('',#4065,#4066,#2692,.T.);
#5306=EDGE_CURVE('',#4066,#4066,#1580,.T.);
#5307=EDGE_CURVE('',#4067,#4068,#2693,.T.);
#5308=EDGE_CURVE('',#4068,#4069,#2147,.T.);
#5309=EDGE_CURVE('',#4070,#4069,#1581,.F.);
#5310=EDGE_CURVE('',#4070,#4067,#2148,.T.);
#5311=EDGE_CURVE('',#4071,#4072,#2694,.T.);
#5312=EDGE_CURVE('',#4072,#4068,#2149,.T.);
#5313=EDGE_CURVE('',#4067,#4071,#2150,.T.);
#5314=EDGE_CURVE('',#4073,#4074,#2695,.T.);
#5315=EDGE_CURVE('',#4074,#4072,#2151,.T.);
#5316=EDGE_CURVE('',#4071,#4073,#2152,.T.);
#5317=EDGE_CURVE('',#4075,#4076,#2696,.T.);
#5318=EDGE_CURVE('',#4076,#4074,#2153,.T.);
#5319=EDGE_CURVE('',#4073,#4075,#2154,.T.);
#5320=EDGE_CURVE('',#4077,#4078,#2697,.T.);
#5321=EDGE_CURVE('',#4077,#4079,#2155,.T.);
#5322=EDGE_CURVE('',#4080,#4079,#1582,.T.);
#5323=EDGE_CURVE('',#4080,#4078,#2156,.T.);
#5324=EDGE_CURVE('',#4081,#4082,#2698,.T.);
#5325=EDGE_CURVE('',#4082,#4083,#2157,.T.);
#5326=EDGE_CURVE('',#4084,#4083,#1583,.T.);
#5327=EDGE_CURVE('',#4081,#4084,#2158,.T.);
#5328=EDGE_CURVE('',#4085,#4086,#2699,.T.);
#5329=EDGE_CURVE('',#4086,#4082,#2159,.T.);
#5330=EDGE_CURVE('',#4085,#4081,#2160,.T.);
#5331=EDGE_CURVE('',#4087,#4088,#2700,.T.);
#5332=EDGE_CURVE('',#4088,#4086,#2161,.T.);
#5333=EDGE_CURVE('',#4087,#4085,#2162,.T.);
#5334=EDGE_CURVE('',#4089,#4090,#2701,.T.);
#5335=EDGE_CURVE('',#4090,#4088,#2163,.T.);
#5336=EDGE_CURVE('',#4089,#4087,#2164,.T.);
#5337=EDGE_CURVE('',#4091,#4092,#2702,.T.);
#5338=EDGE_CURVE('',#4093,#4091,#2165,.T.);
#5339=EDGE_CURVE('',#4094,#4093,#1584,.T.);
#5340=EDGE_CURVE('',#4094,#4092,#2166,.T.);
#5341=EDGE_CURVE('',#4092,#4090,#2167,.T.);
#5342=EDGE_CURVE('',#4091,#4089,#2168,.T.);
#5343=EDGE_CURVE('',#4083,#4070,#2169,.T.);
#5344=EDGE_CURVE('',#4079,#4094,#2170,.T.);
#5345=EDGE_CURVE('',#4075,#4077,#2171,.T.);
#5346=EDGE_CURVE('',#4069,#4084,#2172,.T.);
#5347=EDGE_CURVE('',#4078,#4076,#2173,.T.);
#5348=EDGE_CURVE('',#4093,#4080,#2174,.T.);
#5349=EDGE_CURVE('',#4095,#4096,#2703,.T.);
#5350=EDGE_CURVE('',#4096,#4097,#2704,.T.);
#5351=EDGE_CURVE('',#4097,#4098,#2705,.T.);
#5352=EDGE_CURVE('',#4098,#4099,#2706,.T.);
#5353=EDGE_CURVE('',#4099,#4100,#2707,.T.);
#5354=EDGE_CURVE('',#4100,#4095,#2708,.T.);
#5355=EDGE_CURVE('',#4101,#4102,#2709,.T.);
#5356=EDGE_CURVE('',#4102,#4095,#2710,.T.);
#5357=EDGE_CURVE('',#4101,#4100,#2711,.T.);
#5358=EDGE_CURVE('',#4103,#4101,#2712,.T.);
#5359=EDGE_CURVE('',#4103,#4099,#2713,.T.);
#5360=EDGE_CURVE('',#4104,#4103,#2714,.T.);
#5361=EDGE_CURVE('',#4104,#4098,#2715,.T.);
#5362=EDGE_CURVE('',#4105,#4104,#2716,.T.);
#5363=EDGE_CURVE('',#4105,#4097,#2717,.T.);
#5364=EDGE_CURVE('',#4106,#4105,#2718,.T.);
#5365=EDGE_CURVE('',#4106,#4096,#2719,.T.);
#5366=EDGE_CURVE('',#4102,#4106,#2720,.T.);
#5367=ORIENTED_EDGE('',*,*,#4107,.T.);
#5368=ORIENTED_EDGE('',*,*,#4108,.T.);
#5369=ORIENTED_EDGE('',*,*,#4109,.T.);
#5370=ORIENTED_EDGE('',*,*,#4110,.T.);
#5371=ORIENTED_EDGE('',*,*,#4111,.T.);
#5372=ORIENTED_EDGE('',*,*,#4110,.F.);
#5373=ORIENTED_EDGE('',*,*,#4112,.T.);
#5374=ORIENTED_EDGE('',*,*,#4113,.T.);
#5375=ORIENTED_EDGE('',*,*,#4114,.T.);
#5376=ORIENTED_EDGE('',*,*,#4115,.T.);
#5377=ORIENTED_EDGE('',*,*,#4107,.F.);
#5378=ORIENTED_EDGE('',*,*,#4116,.T.);
#5379=ORIENTED_EDGE('',*,*,#4117,.T.);
#5380=ORIENTED_EDGE('',*,*,#4118,.T.);
#5381=ORIENTED_EDGE('',*,*,#4114,.F.);
#5382=ORIENTED_EDGE('',*,*,#4119,.T.);
#5383=ORIENTED_EDGE('',*,*,#4120,.T.);
#5384=ORIENTED_EDGE('',*,*,#4121,.T.);
#5385=ORIENTED_EDGE('',*,*,#4117,.F.);
#5386=ORIENTED_EDGE('',*,*,#4122,.T.);
#5387=ORIENTED_EDGE('',*,*,#4123,.T.);
#5388=ORIENTED_EDGE('',*,*,#4124,.T.);
#5389=ORIENTED_EDGE('',*,*,#4120,.F.);
#5390=ORIENTED_EDGE('',*,*,#4125,.T.);
#5391=ORIENTED_EDGE('',*,*,#4126,.T.);
#5392=ORIENTED_EDGE('',*,*,#4127,.T.);
#5393=ORIENTED_EDGE('',*,*,#4123,.F.);
#5394=ORIENTED_EDGE('',*,*,#4128,.T.);
#5395=ORIENTED_EDGE('',*,*,#4129,.T.);
#5396=ORIENTED_EDGE('',*,*,#4130,.T.);
#5397=ORIENTED_EDGE('',*,*,#4126,.F.);
#5398=ORIENTED_EDGE('',*,*,#4131,.T.);
#5399=ORIENTED_EDGE('',*,*,#4132,.T.);
#5400=ORIENTED_EDGE('',*,*,#4133,.T.);
#5401=ORIENTED_EDGE('',*,*,#4129,.F.);
#5402=ORIENTED_EDGE('',*,*,#4134,.T.);
#5403=ORIENTED_EDGE('',*,*,#4135,.T.);
#5404=ORIENTED_EDGE('',*,*,#4136,.T.);
#5405=ORIENTED_EDGE('',*,*,#4132,.F.);
#5406=ORIENTED_EDGE('',*,*,#4137,.T.);
#5407=ORIENTED_EDGE('',*,*,#4138,.T.);
#5408=ORIENTED_EDGE('',*,*,#4139,.T.);
#5409=ORIENTED_EDGE('',*,*,#4135,.F.);
#5410=ORIENTED_EDGE('',*,*,#4140,.T.);
#5411=ORIENTED_EDGE('',*,*,#4141,.T.);
#5412=ORIENTED_EDGE('',*,*,#4142,.T.);
#5413=ORIENTED_EDGE('',*,*,#4138,.F.);
#5414=ORIENTED_EDGE('',*,*,#4143,.T.);
#5415=ORIENTED_EDGE('',*,*,#4144,.T.);
#5416=ORIENTED_EDGE('',*,*,#4145,.T.);
#5417=ORIENTED_EDGE('',*,*,#4141,.F.);
#5418=ORIENTED_EDGE('',*,*,#4146,.T.);
#5419=ORIENTED_EDGE('',*,*,#4147,.T.);
#5420=ORIENTED_EDGE('',*,*,#4148,.T.);
#5421=ORIENTED_EDGE('',*,*,#4144,.F.);
#5422=ORIENTED_EDGE('',*,*,#4149,.T.);
#5423=ORIENTED_EDGE('',*,*,#4150,.T.);
#5424=ORIENTED_EDGE('',*,*,#4151,.T.);
#5425=ORIENTED_EDGE('',*,*,#4147,.F.);
#5426=ORIENTED_EDGE('',*,*,#4152,.T.);
#5427=ORIENTED_EDGE('',*,*,#4153,.T.);
#5428=ORIENTED_EDGE('',*,*,#4154,.T.);
#5429=ORIENTED_EDGE('',*,*,#4150,.F.);
#5430=ORIENTED_EDGE('',*,*,#4155,.T.);
#5431=ORIENTED_EDGE('',*,*,#4156,.T.);
#5432=ORIENTED_EDGE('',*,*,#4157,.T.);
#5433=ORIENTED_EDGE('',*,*,#4153,.F.);
#5434=ORIENTED_EDGE('',*,*,#4158,.T.);
#5435=ORIENTED_EDGE('',*,*,#4159,.F.);
#5436=ORIENTED_EDGE('',*,*,#4160,.T.);
#5437=ORIENTED_EDGE('',*,*,#4161,.F.);
#5438=ORIENTED_EDGE('',*,*,#4162,.T.);
#5439=ORIENTED_EDGE('',*,*,#4163,.T.);
#5440=ORIENTED_EDGE('',*,*,#4164,.T.);
#5441=ORIENTED_EDGE('',*,*,#4165,.F.);
#5442=ORIENTED_EDGE('',*,*,#4166,.F.);
#5443=ORIENTED_EDGE('',*,*,#4167,.T.);
#5444=ORIENTED_EDGE('',*,*,#4168,.T.);
#5445=ORIENTED_EDGE('',*,*,#4163,.F.);
#5446=ORIENTED_EDGE('',*,*,#4169,.F.);
#5447=ORIENTED_EDGE('',*,*,#4170,.T.);
#5448=ORIENTED_EDGE('',*,*,#4171,.T.);
#5449=ORIENTED_EDGE('',*,*,#4167,.F.);
#5450=ORIENTED_EDGE('',*,*,#4172,.F.);
#5451=ORIENTED_EDGE('',*,*,#4173,.T.);
#5452=ORIENTED_EDGE('',*,*,#4174,.T.);
#5453=ORIENTED_EDGE('',*,*,#4170,.F.);
#5454=ORIENTED_EDGE('',*,*,#4175,.F.);
#5455=ORIENTED_EDGE('',*,*,#4176,.T.);
#5456=ORIENTED_EDGE('',*,*,#4177,.T.);
#5457=ORIENTED_EDGE('',*,*,#4173,.F.);
#5458=ORIENTED_EDGE('',*,*,#4178,.F.);
#5459=ORIENTED_EDGE('',*,*,#4179,.T.);
#5460=ORIENTED_EDGE('',*,*,#4180,.T.);
#5461=ORIENTED_EDGE('',*,*,#4176,.F.);
#5462=ORIENTED_EDGE('',*,*,#4181,.F.);
#5463=ORIENTED_EDGE('',*,*,#4182,.T.);
#5464=ORIENTED_EDGE('',*,*,#4183,.T.);
#5465=ORIENTED_EDGE('',*,*,#4179,.F.);
#5466=ORIENTED_EDGE('',*,*,#4184,.F.);
#5467=ORIENTED_EDGE('',*,*,#4185,.T.);
#5468=ORIENTED_EDGE('',*,*,#4186,.T.);
#5469=ORIENTED_EDGE('',*,*,#4182,.F.);
#5470=ORIENTED_EDGE('',*,*,#4187,.F.);
#5471=ORIENTED_EDGE('',*,*,#4188,.T.);
#5472=ORIENTED_EDGE('',*,*,#4189,.T.);
#5473=ORIENTED_EDGE('',*,*,#4185,.F.);
#5474=ORIENTED_EDGE('',*,*,#4190,.F.);
#5475=ORIENTED_EDGE('',*,*,#4191,.T.);
#5476=ORIENTED_EDGE('',*,*,#4192,.T.);
#5477=ORIENTED_EDGE('',*,*,#4188,.F.);
#5478=ORIENTED_EDGE('',*,*,#4193,.F.);
#5479=ORIENTED_EDGE('',*,*,#4194,.T.);
#5480=ORIENTED_EDGE('',*,*,#4195,.T.);
#5481=ORIENTED_EDGE('',*,*,#4191,.F.);
#5482=ORIENTED_EDGE('',*,*,#4196,.F.);
#5483=ORIENTED_EDGE('',*,*,#4197,.T.);
#5484=ORIENTED_EDGE('',*,*,#4198,.T.);
#5485=ORIENTED_EDGE('',*,*,#4194,.F.);
#5486=ORIENTED_EDGE('',*,*,#4199,.F.);
#5487=ORIENTED_EDGE('',*,*,#4200,.T.);
#5488=ORIENTED_EDGE('',*,*,#4201,.T.);
#5489=ORIENTED_EDGE('',*,*,#4197,.F.);
#5490=ORIENTED_EDGE('',*,*,#4202,.F.);
#5491=ORIENTED_EDGE('',*,*,#4203,.T.);
#5492=ORIENTED_EDGE('',*,*,#4204,.T.);
#5493=ORIENTED_EDGE('',*,*,#4200,.F.);
#5494=ORIENTED_EDGE('',*,*,#4205,.F.);
#5495=ORIENTED_EDGE('',*,*,#4206,.T.);
#5496=ORIENTED_EDGE('',*,*,#4207,.T.);
#5497=ORIENTED_EDGE('',*,*,#4203,.F.);
#5498=ORIENTED_EDGE('',*,*,#4208,.F.);
#5499=ORIENTED_EDGE('',*,*,#4209,.T.);
#5500=ORIENTED_EDGE('',*,*,#4210,.T.);
#5501=ORIENTED_EDGE('',*,*,#4206,.F.);
#5502=ORIENTED_EDGE('',*,*,#4211,.F.);
#5503=ORIENTED_EDGE('',*,*,#4212,.F.);
#5504=ORIENTED_EDGE('',*,*,#4213,.F.);
#5505=ORIENTED_EDGE('',*,*,#4214,.F.);
#5506=ORIENTED_EDGE('',*,*,#4215,.T.);
#5507=ORIENTED_EDGE('',*,*,#4216,.T.);
#5508=ORIENTED_EDGE('',*,*,#4217,.T.);
#5509=ORIENTED_EDGE('',*,*,#4218,.T.);
#5510=ORIENTED_EDGE('',*,*,#4219,.T.);
#5511=ORIENTED_EDGE('',*,*,#4220,.T.);
#5512=ORIENTED_EDGE('',*,*,#4219,.F.);
#5513=ORIENTED_EDGE('',*,*,#4221,.T.);
#5514=ORIENTED_EDGE('',*,*,#4222,.T.);
#5515=ORIENTED_EDGE('',*,*,#4223,.T.);
#5516=ORIENTED_EDGE('',*,*,#4224,.T.);
#5517=ORIENTED_EDGE('',*,*,#4216,.F.);
#5518=ORIENTED_EDGE('',*,*,#4225,.T.);
#5519=ORIENTED_EDGE('',*,*,#4226,.T.);
#5520=ORIENTED_EDGE('',*,*,#4227,.T.);
#5521=ORIENTED_EDGE('',*,*,#4223,.F.);
#5522=ORIENTED_EDGE('',*,*,#4228,.T.);
#5523=ORIENTED_EDGE('',*,*,#4229,.T.);
#5524=ORIENTED_EDGE('',*,*,#4230,.T.);
#5525=ORIENTED_EDGE('',*,*,#4226,.F.);
#5526=ORIENTED_EDGE('',*,*,#4231,.T.);
#5527=ORIENTED_EDGE('',*,*,#4232,.T.);
#5528=ORIENTED_EDGE('',*,*,#4233,.T.);
#5529=ORIENTED_EDGE('',*,*,#4229,.F.);
#5530=ORIENTED_EDGE('',*,*,#4234,.T.);
#5531=ORIENTED_EDGE('',*,*,#4235,.T.);
#5532=ORIENTED_EDGE('',*,*,#4236,.T.);
#5533=ORIENTED_EDGE('',*,*,#4232,.F.);
#5534=ORIENTED_EDGE('',*,*,#4237,.T.);
#5535=ORIENTED_EDGE('',*,*,#4238,.T.);
#5536=ORIENTED_EDGE('',*,*,#4239,.T.);
#5537=ORIENTED_EDGE('',*,*,#4235,.F.);
#5538=ORIENTED_EDGE('',*,*,#4240,.T.);
#5539=ORIENTED_EDGE('',*,*,#4241,.T.);
#5540=ORIENTED_EDGE('',*,*,#4242,.T.);
#5541=ORIENTED_EDGE('',*,*,#4238,.F.);
#5542=ORIENTED_EDGE('',*,*,#4243,.T.);
#5543=ORIENTED_EDGE('',*,*,#4244,.T.);
#5544=ORIENTED_EDGE('',*,*,#4245,.T.);
#5545=ORIENTED_EDGE('',*,*,#4241,.F.);
#5546=ORIENTED_EDGE('',*,*,#4246,.T.);
#5547=ORIENTED_EDGE('',*,*,#4247,.T.);
#5548=ORIENTED_EDGE('',*,*,#4248,.T.);
#5549=ORIENTED_EDGE('',*,*,#4244,.F.);
#5550=ORIENTED_EDGE('',*,*,#4249,.T.);
#5551=ORIENTED_EDGE('',*,*,#4250,.T.);
#5552=ORIENTED_EDGE('',*,*,#4251,.T.);
#5553=ORIENTED_EDGE('',*,*,#4247,.F.);
#5554=ORIENTED_EDGE('',*,*,#4252,.T.);
#5555=ORIENTED_EDGE('',*,*,#4253,.T.);
#5556=ORIENTED_EDGE('',*,*,#4254,.T.);
#5557=ORIENTED_EDGE('',*,*,#4250,.F.);
#5558=ORIENTED_EDGE('',*,*,#4255,.T.);
#5559=ORIENTED_EDGE('',*,*,#4256,.T.);
#5560=ORIENTED_EDGE('',*,*,#4257,.T.);
#5561=ORIENTED_EDGE('',*,*,#4253,.F.);
#5562=ORIENTED_EDGE('',*,*,#4258,.T.);
#5563=ORIENTED_EDGE('',*,*,#4259,.T.);
#5564=ORIENTED_EDGE('',*,*,#4260,.T.);
#5565=ORIENTED_EDGE('',*,*,#4256,.F.);
#5566=ORIENTED_EDGE('',*,*,#4261,.T.);
#5567=ORIENTED_EDGE('',*,*,#4262,.T.);
#5568=ORIENTED_EDGE('',*,*,#4263,.T.);
#5569=ORIENTED_EDGE('',*,*,#4259,.F.);
#5570=ORIENTED_EDGE('',*,*,#4264,.T.);
#5571=ORIENTED_EDGE('',*,*,#4265,.T.);
#5572=ORIENTED_EDGE('',*,*,#4266,.T.);
#5573=ORIENTED_EDGE('',*,*,#4262,.F.);
#5574=ORIENTED_EDGE('',*,*,#4267,.T.);
#5575=ORIENTED_EDGE('',*,*,#4268,.F.);
#5576=ORIENTED_EDGE('',*,*,#4269,.T.);
#5577=ORIENTED_EDGE('',*,*,#4270,.F.);
#5578=ORIENTED_EDGE('',*,*,#4271,.T.);
#5579=ORIENTED_EDGE('',*,*,#4272,.T.);
#5580=ORIENTED_EDGE('',*,*,#4273,.T.);
#5581=ORIENTED_EDGE('',*,*,#4274,.F.);
#5582=ORIENTED_EDGE('',*,*,#4275,.F.);
#5583=ORIENTED_EDGE('',*,*,#4276,.T.);
#5584=ORIENTED_EDGE('',*,*,#4277,.T.);
#5585=ORIENTED_EDGE('',*,*,#4272,.F.);
#5586=ORIENTED_EDGE('',*,*,#4278,.F.);
#5587=ORIENTED_EDGE('',*,*,#4279,.T.);
#5588=ORIENTED_EDGE('',*,*,#4280,.T.);
#5589=ORIENTED_EDGE('',*,*,#4276,.F.);
#5590=ORIENTED_EDGE('',*,*,#4281,.F.);
#5591=ORIENTED_EDGE('',*,*,#4282,.T.);
#5592=ORIENTED_EDGE('',*,*,#4283,.T.);
#5593=ORIENTED_EDGE('',*,*,#4279,.F.);
#5594=ORIENTED_EDGE('',*,*,#4284,.F.);
#5595=ORIENTED_EDGE('',*,*,#4285,.T.);
#5596=ORIENTED_EDGE('',*,*,#4286,.T.);
#5597=ORIENTED_EDGE('',*,*,#4282,.F.);
#5598=ORIENTED_EDGE('',*,*,#4287,.F.);
#5599=ORIENTED_EDGE('',*,*,#4288,.T.);
#5600=ORIENTED_EDGE('',*,*,#4289,.T.);
#5601=ORIENTED_EDGE('',*,*,#4285,.F.);
#5602=ORIENTED_EDGE('',*,*,#4290,.F.);
#5603=ORIENTED_EDGE('',*,*,#4291,.T.);
#5604=ORIENTED_EDGE('',*,*,#4292,.T.);
#5605=ORIENTED_EDGE('',*,*,#4288,.F.);
#5606=ORIENTED_EDGE('',*,*,#4293,.F.);
#5607=ORIENTED_EDGE('',*,*,#4294,.T.);
#5608=ORIENTED_EDGE('',*,*,#4295,.T.);
#5609=ORIENTED_EDGE('',*,*,#4291,.F.);
#5610=ORIENTED_EDGE('',*,*,#4296,.F.);
#5611=ORIENTED_EDGE('',*,*,#4297,.T.);
#5612=ORIENTED_EDGE('',*,*,#4298,.T.);
#5613=ORIENTED_EDGE('',*,*,#4294,.F.);
#5614=ORIENTED_EDGE('',*,*,#4299,.F.);
#5615=ORIENTED_EDGE('',*,*,#4300,.T.);
#5616=ORIENTED_EDGE('',*,*,#4301,.T.);
#5617=ORIENTED_EDGE('',*,*,#4297,.F.);
#5618=ORIENTED_EDGE('',*,*,#4302,.F.);
#5619=ORIENTED_EDGE('',*,*,#4303,.T.);
#5620=ORIENTED_EDGE('',*,*,#4304,.T.);
#5621=ORIENTED_EDGE('',*,*,#4300,.F.);
#5622=ORIENTED_EDGE('',*,*,#4305,.F.);
#5623=ORIENTED_EDGE('',*,*,#4306,.T.);
#5624=ORIENTED_EDGE('',*,*,#4307,.T.);
#5625=ORIENTED_EDGE('',*,*,#4303,.F.);
#5626=ORIENTED_EDGE('',*,*,#4308,.F.);
#5627=ORIENTED_EDGE('',*,*,#4309,.T.);
#5628=ORIENTED_EDGE('',*,*,#4310,.T.);
#5629=ORIENTED_EDGE('',*,*,#4306,.F.);
#5630=ORIENTED_EDGE('',*,*,#4311,.F.);
#5631=ORIENTED_EDGE('',*,*,#4312,.T.);
#5632=ORIENTED_EDGE('',*,*,#4313,.T.);
#5633=ORIENTED_EDGE('',*,*,#4309,.F.);
#5634=ORIENTED_EDGE('',*,*,#4314,.F.);
#5635=ORIENTED_EDGE('',*,*,#4315,.T.);
#5636=ORIENTED_EDGE('',*,*,#4316,.T.);
#5637=ORIENTED_EDGE('',*,*,#4312,.F.);
#5638=ORIENTED_EDGE('',*,*,#4317,.F.);
#5639=ORIENTED_EDGE('',*,*,#4318,.T.);
#5640=ORIENTED_EDGE('',*,*,#4319,.T.);
#5641=ORIENTED_EDGE('',*,*,#4315,.F.);
#5642=ORIENTED_EDGE('',*,*,#4320,.F.);
#5643=ORIENTED_EDGE('',*,*,#4321,.F.);
#5644=ORIENTED_EDGE('',*,*,#4322,.F.);
#5645=ORIENTED_EDGE('',*,*,#4323,.F.);
#5646=ORIENTED_EDGE('',*,*,#4324,.T.);
#5647=ORIENTED_EDGE('',*,*,#4325,.T.);
#5648=ORIENTED_EDGE('',*,*,#4326,.T.);
#5649=ORIENTED_EDGE('',*,*,#4327,.T.);
#5650=ORIENTED_EDGE('',*,*,#4328,.T.);
#5651=ORIENTED_EDGE('',*,*,#4329,.T.);
#5652=ORIENTED_EDGE('',*,*,#4328,.F.);
#5653=ORIENTED_EDGE('',*,*,#4330,.T.);
#5654=ORIENTED_EDGE('',*,*,#4331,.T.);
#5655=ORIENTED_EDGE('',*,*,#4332,.T.);
#5656=ORIENTED_EDGE('',*,*,#4333,.T.);
#5657=ORIENTED_EDGE('',*,*,#4325,.F.);
#5658=ORIENTED_EDGE('',*,*,#4334,.T.);
#5659=ORIENTED_EDGE('',*,*,#4335,.T.);
#5660=ORIENTED_EDGE('',*,*,#4336,.T.);
#5661=ORIENTED_EDGE('',*,*,#4332,.F.);
#5662=ORIENTED_EDGE('',*,*,#4337,.T.);
#5663=ORIENTED_EDGE('',*,*,#4338,.T.);
#5664=ORIENTED_EDGE('',*,*,#4339,.T.);
#5665=ORIENTED_EDGE('',*,*,#4335,.F.);
#5666=ORIENTED_EDGE('',*,*,#4340,.T.);
#5667=ORIENTED_EDGE('',*,*,#4341,.T.);
#5668=ORIENTED_EDGE('',*,*,#4342,.T.);
#5669=ORIENTED_EDGE('',*,*,#4338,.F.);
#5670=ORIENTED_EDGE('',*,*,#4343,.T.);
#5671=ORIENTED_EDGE('',*,*,#4344,.T.);
#5672=ORIENTED_EDGE('',*,*,#4345,.T.);
#5673=ORIENTED_EDGE('',*,*,#4341,.F.);
#5674=ORIENTED_EDGE('',*,*,#4346,.T.);
#5675=ORIENTED_EDGE('',*,*,#4347,.T.);
#5676=ORIENTED_EDGE('',*,*,#4348,.T.);
#5677=ORIENTED_EDGE('',*,*,#4344,.F.);
#5678=ORIENTED_EDGE('',*,*,#4349,.T.);
#5679=ORIENTED_EDGE('',*,*,#4350,.T.);
#5680=ORIENTED_EDGE('',*,*,#4351,.T.);
#5681=ORIENTED_EDGE('',*,*,#4347,.F.);
#5682=ORIENTED_EDGE('',*,*,#4352,.T.);
#5683=ORIENTED_EDGE('',*,*,#4353,.T.);
#5684=ORIENTED_EDGE('',*,*,#4354,.T.);
#5685=ORIENTED_EDGE('',*,*,#4350,.F.);
#5686=ORIENTED_EDGE('',*,*,#4355,.T.);
#5687=ORIENTED_EDGE('',*,*,#4356,.T.);
#5688=ORIENTED_EDGE('',*,*,#4357,.T.);
#5689=ORIENTED_EDGE('',*,*,#4353,.F.);
#5690=ORIENTED_EDGE('',*,*,#4358,.T.);
#5691=ORIENTED_EDGE('',*,*,#4359,.T.);
#5692=ORIENTED_EDGE('',*,*,#4360,.T.);
#5693=ORIENTED_EDGE('',*,*,#4356,.F.);
#5694=ORIENTED_EDGE('',*,*,#4361,.T.);
#5695=ORIENTED_EDGE('',*,*,#4362,.T.);
#5696=ORIENTED_EDGE('',*,*,#4363,.T.);
#5697=ORIENTED_EDGE('',*,*,#4359,.F.);
#5698=ORIENTED_EDGE('',*,*,#4364,.T.);
#5699=ORIENTED_EDGE('',*,*,#4365,.T.);
#5700=ORIENTED_EDGE('',*,*,#4366,.T.);
#5701=ORIENTED_EDGE('',*,*,#4362,.F.);
#5702=ORIENTED_EDGE('',*,*,#4367,.T.);
#5703=ORIENTED_EDGE('',*,*,#4368,.T.);
#5704=ORIENTED_EDGE('',*,*,#4369,.T.);
#5705=ORIENTED_EDGE('',*,*,#4365,.F.);
#5706=ORIENTED_EDGE('',*,*,#4370,.T.);
#5707=ORIENTED_EDGE('',*,*,#4371,.T.);
#5708=ORIENTED_EDGE('',*,*,#4372,.T.);
#5709=ORIENTED_EDGE('',*,*,#4368,.F.);
#5710=ORIENTED_EDGE('',*,*,#4373,.T.);
#5711=ORIENTED_EDGE('',*,*,#4374,.T.);
#5712=ORIENTED_EDGE('',*,*,#4375,.T.);
#5713=ORIENTED_EDGE('',*,*,#4371,.F.);
#5714=ORIENTED_EDGE('',*,*,#4376,.T.);
#5715=ORIENTED_EDGE('',*,*,#4377,.F.);
#5716=ORIENTED_EDGE('',*,*,#4378,.T.);
#5717=ORIENTED_EDGE('',*,*,#4379,.F.);
#5718=ORIENTED_EDGE('',*,*,#4380,.T.);
#5719=ORIENTED_EDGE('',*,*,#4381,.T.);
#5720=ORIENTED_EDGE('',*,*,#4382,.T.);
#5721=ORIENTED_EDGE('',*,*,#4383,.F.);
#5722=ORIENTED_EDGE('',*,*,#4384,.F.);
#5723=ORIENTED_EDGE('',*,*,#4385,.T.);
#5724=ORIENTED_EDGE('',*,*,#4386,.T.);
#5725=ORIENTED_EDGE('',*,*,#4381,.F.);
#5726=ORIENTED_EDGE('',*,*,#4387,.F.);
#5727=ORIENTED_EDGE('',*,*,#4388,.T.);
#5728=ORIENTED_EDGE('',*,*,#4389,.T.);
#5729=ORIENTED_EDGE('',*,*,#4385,.F.);
#5730=ORIENTED_EDGE('',*,*,#4390,.F.);
#5731=ORIENTED_EDGE('',*,*,#4391,.T.);
#5732=ORIENTED_EDGE('',*,*,#4392,.T.);
#5733=ORIENTED_EDGE('',*,*,#4388,.F.);
#5734=ORIENTED_EDGE('',*,*,#4393,.F.);
#5735=ORIENTED_EDGE('',*,*,#4394,.T.);
#5736=ORIENTED_EDGE('',*,*,#4395,.T.);
#5737=ORIENTED_EDGE('',*,*,#4391,.F.);
#5738=ORIENTED_EDGE('',*,*,#4396,.F.);
#5739=ORIENTED_EDGE('',*,*,#4397,.T.);
#5740=ORIENTED_EDGE('',*,*,#4398,.T.);
#5741=ORIENTED_EDGE('',*,*,#4394,.F.);
#5742=ORIENTED_EDGE('',*,*,#4399,.F.);
#5743=ORIENTED_EDGE('',*,*,#4400,.T.);
#5744=ORIENTED_EDGE('',*,*,#4401,.T.);
#5745=ORIENTED_EDGE('',*,*,#4397,.F.);
#5746=ORIENTED_EDGE('',*,*,#4402,.F.);
#5747=ORIENTED_EDGE('',*,*,#4403,.T.);
#5748=ORIENTED_EDGE('',*,*,#4404,.T.);
#5749=ORIENTED_EDGE('',*,*,#4400,.F.);
#5750=ORIENTED_EDGE('',*,*,#4405,.F.);
#5751=ORIENTED_EDGE('',*,*,#4406,.T.);
#5752=ORIENTED_EDGE('',*,*,#4407,.T.);
#5753=ORIENTED_EDGE('',*,*,#4403,.F.);
#5754=ORIENTED_EDGE('',*,*,#4408,.F.);
#5755=ORIENTED_EDGE('',*,*,#4409,.T.);
#5756=ORIENTED_EDGE('',*,*,#4410,.T.);
#5757=ORIENTED_EDGE('',*,*,#4406,.F.);
#5758=ORIENTED_EDGE('',*,*,#4411,.F.);
#5759=ORIENTED_EDGE('',*,*,#4412,.T.);
#5760=ORIENTED_EDGE('',*,*,#4413,.T.);
#5761=ORIENTED_EDGE('',*,*,#4409,.F.);
#5762=ORIENTED_EDGE('',*,*,#4414,.F.);
#5763=ORIENTED_EDGE('',*,*,#4415,.T.);
#5764=ORIENTED_EDGE('',*,*,#4416,.T.);
#5765=ORIENTED_EDGE('',*,*,#4412,.F.);
#5766=ORIENTED_EDGE('',*,*,#4417,.F.);
#5767=ORIENTED_EDGE('',*,*,#4418,.T.);
#5768=ORIENTED_EDGE('',*,*,#4419,.T.);
#5769=ORIENTED_EDGE('',*,*,#4415,.F.);
#5770=ORIENTED_EDGE('',*,*,#4420,.F.);
#5771=ORIENTED_EDGE('',*,*,#4421,.T.);
#5772=ORIENTED_EDGE('',*,*,#4422,.T.);
#5773=ORIENTED_EDGE('',*,*,#4418,.F.);
#5774=ORIENTED_EDGE('',*,*,#4423,.F.);
#5775=ORIENTED_EDGE('',*,*,#4424,.T.);
#5776=ORIENTED_EDGE('',*,*,#4425,.T.);
#5777=ORIENTED_EDGE('',*,*,#4421,.F.);
#5778=ORIENTED_EDGE('',*,*,#4426,.F.);
#5779=ORIENTED_EDGE('',*,*,#4427,.T.);
#5780=ORIENTED_EDGE('',*,*,#4428,.T.);
#5781=ORIENTED_EDGE('',*,*,#4424,.F.);
#5782=ORIENTED_EDGE('',*,*,#4429,.F.);
#5783=ORIENTED_EDGE('',*,*,#4430,.F.);
#5784=ORIENTED_EDGE('',*,*,#4431,.F.);
#5785=ORIENTED_EDGE('',*,*,#4432,.F.);
#5786=ORIENTED_EDGE('',*,*,#4433,.T.);
#5787=ORIENTED_EDGE('',*,*,#4434,.T.);
#5788=ORIENTED_EDGE('',*,*,#4435,.T.);
#5789=ORIENTED_EDGE('',*,*,#4436,.T.);
#5790=ORIENTED_EDGE('',*,*,#4437,.T.);
#5791=ORIENTED_EDGE('',*,*,#4438,.T.);
#5792=ORIENTED_EDGE('',*,*,#4437,.F.);
#5793=ORIENTED_EDGE('',*,*,#4439,.T.);
#5794=ORIENTED_EDGE('',*,*,#4440,.T.);
#5795=ORIENTED_EDGE('',*,*,#4441,.T.);
#5796=ORIENTED_EDGE('',*,*,#4442,.T.);
#5797=ORIENTED_EDGE('',*,*,#4434,.F.);
#5798=ORIENTED_EDGE('',*,*,#4443,.T.);
#5799=ORIENTED_EDGE('',*,*,#4444,.T.);
#5800=ORIENTED_EDGE('',*,*,#4445,.T.);
#5801=ORIENTED_EDGE('',*,*,#4441,.F.);
#5802=ORIENTED_EDGE('',*,*,#4446,.T.);
#5803=ORIENTED_EDGE('',*,*,#4447,.T.);
#5804=ORIENTED_EDGE('',*,*,#4448,.T.);
#5805=ORIENTED_EDGE('',*,*,#4444,.F.);
#5806=ORIENTED_EDGE('',*,*,#4449,.T.);
#5807=ORIENTED_EDGE('',*,*,#4450,.T.);
#5808=ORIENTED_EDGE('',*,*,#4451,.T.);
#5809=ORIENTED_EDGE('',*,*,#4447,.F.);
#5810=ORIENTED_EDGE('',*,*,#4452,.T.);
#5811=ORIENTED_EDGE('',*,*,#4453,.T.);
#5812=ORIENTED_EDGE('',*,*,#4454,.T.);
#5813=ORIENTED_EDGE('',*,*,#4450,.F.);
#5814=ORIENTED_EDGE('',*,*,#4455,.T.);
#5815=ORIENTED_EDGE('',*,*,#4456,.T.);
#5816=ORIENTED_EDGE('',*,*,#4457,.T.);
#5817=ORIENTED_EDGE('',*,*,#4453,.F.);
#5818=ORIENTED_EDGE('',*,*,#4458,.T.);
#5819=ORIENTED_EDGE('',*,*,#4459,.T.);
#5820=ORIENTED_EDGE('',*,*,#4460,.T.);
#5821=ORIENTED_EDGE('',*,*,#4456,.F.);
#5822=ORIENTED_EDGE('',*,*,#4461,.T.);
#5823=ORIENTED_EDGE('',*,*,#4462,.T.);
#5824=ORIENTED_EDGE('',*,*,#4463,.T.);
#5825=ORIENTED_EDGE('',*,*,#4459,.F.);
#5826=ORIENTED_EDGE('',*,*,#4464,.T.);
#5827=ORIENTED_EDGE('',*,*,#4465,.T.);
#5828=ORIENTED_EDGE('',*,*,#4466,.T.);
#5829=ORIENTED_EDGE('',*,*,#4462,.F.);
#5830=ORIENTED_EDGE('',*,*,#4467,.T.);
#5831=ORIENTED_EDGE('',*,*,#4468,.T.);
#5832=ORIENTED_EDGE('',*,*,#4469,.T.);
#5833=ORIENTED_EDGE('',*,*,#4465,.F.);
#5834=ORIENTED_EDGE('',*,*,#4470,.T.);
#5835=ORIENTED_EDGE('',*,*,#4471,.T.);
#5836=ORIENTED_EDGE('',*,*,#4472,.T.);
#5837=ORIENTED_EDGE('',*,*,#4468,.F.);
#5838=ORIENTED_EDGE('',*,*,#4473,.T.);
#5839=ORIENTED_EDGE('',*,*,#4474,.T.);
#5840=ORIENTED_EDGE('',*,*,#4475,.T.);
#5841=ORIENTED_EDGE('',*,*,#4471,.F.);
#5842=ORIENTED_EDGE('',*,*,#4476,.T.);
#5843=ORIENTED_EDGE('',*,*,#4477,.T.);
#5844=ORIENTED_EDGE('',*,*,#4478,.T.);
#5845=ORIENTED_EDGE('',*,*,#4474,.F.);
#5846=ORIENTED_EDGE('',*,*,#4479,.T.);
#5847=ORIENTED_EDGE('',*,*,#4480,.T.);
#5848=ORIENTED_EDGE('',*,*,#4481,.T.);
#5849=ORIENTED_EDGE('',*,*,#4477,.F.);
#5850=ORIENTED_EDGE('',*,*,#4482,.T.);
#5851=ORIENTED_EDGE('',*,*,#4483,.T.);
#5852=ORIENTED_EDGE('',*,*,#4484,.T.);
#5853=ORIENTED_EDGE('',*,*,#4480,.F.);
#5854=ORIENTED_EDGE('',*,*,#4485,.T.);
#5855=ORIENTED_EDGE('',*,*,#4486,.F.);
#5856=ORIENTED_EDGE('',*,*,#4487,.T.);
#5857=ORIENTED_EDGE('',*,*,#4488,.F.);
#5858=ORIENTED_EDGE('',*,*,#4489,.T.);
#5859=ORIENTED_EDGE('',*,*,#4490,.T.);
#5860=ORIENTED_EDGE('',*,*,#4491,.T.);
#5861=ORIENTED_EDGE('',*,*,#4492,.F.);
#5862=ORIENTED_EDGE('',*,*,#4493,.F.);
#5863=ORIENTED_EDGE('',*,*,#4494,.T.);
#5864=ORIENTED_EDGE('',*,*,#4495,.T.);
#5865=ORIENTED_EDGE('',*,*,#4490,.F.);
#5866=ORIENTED_EDGE('',*,*,#4496,.F.);
#5867=ORIENTED_EDGE('',*,*,#4497,.T.);
#5868=ORIENTED_EDGE('',*,*,#4498,.T.);
#5869=ORIENTED_EDGE('',*,*,#4494,.F.);
#5870=ORIENTED_EDGE('',*,*,#4499,.F.);
#5871=ORIENTED_EDGE('',*,*,#4500,.T.);
#5872=ORIENTED_EDGE('',*,*,#4501,.T.);
#5873=ORIENTED_EDGE('',*,*,#4497,.F.);
#5874=ORIENTED_EDGE('',*,*,#4502,.F.);
#5875=ORIENTED_EDGE('',*,*,#4503,.T.);
#5876=ORIENTED_EDGE('',*,*,#4504,.T.);
#5877=ORIENTED_EDGE('',*,*,#4500,.F.);
#5878=ORIENTED_EDGE('',*,*,#4505,.F.);
#5879=ORIENTED_EDGE('',*,*,#4506,.T.);
#5880=ORIENTED_EDGE('',*,*,#4507,.T.);
#5881=ORIENTED_EDGE('',*,*,#4503,.F.);
#5882=ORIENTED_EDGE('',*,*,#4508,.F.);
#5883=ORIENTED_EDGE('',*,*,#4509,.T.);
#5884=ORIENTED_EDGE('',*,*,#4510,.T.);
#5885=ORIENTED_EDGE('',*,*,#4506,.F.);
#5886=ORIENTED_EDGE('',*,*,#4511,.F.);
#5887=ORIENTED_EDGE('',*,*,#4512,.T.);
#5888=ORIENTED_EDGE('',*,*,#4513,.T.);
#5889=ORIENTED_EDGE('',*,*,#4509,.F.);
#5890=ORIENTED_EDGE('',*,*,#4514,.F.);
#5891=ORIENTED_EDGE('',*,*,#4515,.T.);
#5892=ORIENTED_EDGE('',*,*,#4516,.T.);
#5893=ORIENTED_EDGE('',*,*,#4512,.F.);
#5894=ORIENTED_EDGE('',*,*,#4517,.F.);
#5895=ORIENTED_EDGE('',*,*,#4518,.T.);
#5896=ORIENTED_EDGE('',*,*,#4519,.T.);
#5897=ORIENTED_EDGE('',*,*,#4515,.F.);
#5898=ORIENTED_EDGE('',*,*,#4520,.F.);
#5899=ORIENTED_EDGE('',*,*,#4521,.T.);
#5900=ORIENTED_EDGE('',*,*,#4522,.T.);
#5901=ORIENTED_EDGE('',*,*,#4518,.F.);
#5902=ORIENTED_EDGE('',*,*,#4523,.F.);
#5903=ORIENTED_EDGE('',*,*,#4524,.T.);
#5904=ORIENTED_EDGE('',*,*,#4525,.T.);
#5905=ORIENTED_EDGE('',*,*,#4521,.F.);
#5906=ORIENTED_EDGE('',*,*,#4526,.F.);
#5907=ORIENTED_EDGE('',*,*,#4527,.T.);
#5908=ORIENTED_EDGE('',*,*,#4528,.T.);
#5909=ORIENTED_EDGE('',*,*,#4524,.F.);
#5910=ORIENTED_EDGE('',*,*,#4529,.F.);
#5911=ORIENTED_EDGE('',*,*,#4530,.T.);
#5912=ORIENTED_EDGE('',*,*,#4531,.T.);
#5913=ORIENTED_EDGE('',*,*,#4527,.F.);
#5914=ORIENTED_EDGE('',*,*,#4532,.F.);
#5915=ORIENTED_EDGE('',*,*,#4533,.T.);
#5916=ORIENTED_EDGE('',*,*,#4534,.T.);
#5917=ORIENTED_EDGE('',*,*,#4530,.F.);
#5918=ORIENTED_EDGE('',*,*,#4535,.F.);
#5919=ORIENTED_EDGE('',*,*,#4536,.T.);
#5920=ORIENTED_EDGE('',*,*,#4537,.T.);
#5921=ORIENTED_EDGE('',*,*,#4533,.F.);
#5922=ORIENTED_EDGE('',*,*,#4538,.F.);
#5923=ORIENTED_EDGE('',*,*,#4539,.F.);
#5924=ORIENTED_EDGE('',*,*,#4540,.F.);
#5925=ORIENTED_EDGE('',*,*,#4541,.F.);
#5926=ORIENTED_EDGE('',*,*,#4542,.T.);
#5927=ORIENTED_EDGE('',*,*,#4436,.F.);
#5928=ORIENTED_EDGE('',*,*,#4543,.T.);
#5929=ORIENTED_EDGE('',*,*,#4492,.T.);
#5930=ORIENTED_EDGE('',*,*,#4544,.T.);
#5931=ORIENTED_EDGE('',*,*,#4439,.F.);
#5932=ORIENTED_EDGE('',*,*,#4539,.T.);
#5933=ORIENTED_EDGE('',*,*,#4545,.T.);
#5934=ORIENTED_EDGE('',*,*,#4536,.F.);
#5935=ORIENTED_EDGE('',*,*,#4546,.F.);
#5936=ORIENTED_EDGE('',*,*,#4544,.F.);
#5937=ORIENTED_EDGE('',*,*,#4491,.F.);
#5938=ORIENTED_EDGE('',*,*,#4495,.F.);
#5939=ORIENTED_EDGE('',*,*,#4498,.F.);
#5940=ORIENTED_EDGE('',*,*,#4501,.F.);
#5941=ORIENTED_EDGE('',*,*,#4504,.F.);
#5942=ORIENTED_EDGE('',*,*,#4507,.F.);
#5943=ORIENTED_EDGE('',*,*,#4510,.F.);
#5944=ORIENTED_EDGE('',*,*,#4513,.F.);
#5945=ORIENTED_EDGE('',*,*,#4516,.F.);
#5946=ORIENTED_EDGE('',*,*,#4519,.F.);
#5947=ORIENTED_EDGE('',*,*,#4522,.F.);
#5948=ORIENTED_EDGE('',*,*,#4525,.F.);
#5949=ORIENTED_EDGE('',*,*,#4528,.F.);
#5950=ORIENTED_EDGE('',*,*,#4531,.F.);
#5951=ORIENTED_EDGE('',*,*,#4534,.F.);
#5952=ORIENTED_EDGE('',*,*,#4537,.F.);
#5953=ORIENTED_EDGE('',*,*,#4545,.F.);
#5954=ORIENTED_EDGE('',*,*,#4542,.F.);
#5955=ORIENTED_EDGE('',*,*,#4547,.F.);
#5956=ORIENTED_EDGE('',*,*,#4487,.F.);
#5957=ORIENTED_EDGE('',*,*,#4548,.F.);
#5958=ORIENTED_EDGE('',*,*,#4485,.F.);
#5959=ORIENTED_EDGE('',*,*,#4482,.F.);
#5960=ORIENTED_EDGE('',*,*,#4479,.F.);
#5961=ORIENTED_EDGE('',*,*,#4476,.F.);
#5962=ORIENTED_EDGE('',*,*,#4473,.F.);
#5963=ORIENTED_EDGE('',*,*,#4470,.F.);
#5964=ORIENTED_EDGE('',*,*,#4467,.F.);
#5965=ORIENTED_EDGE('',*,*,#4464,.F.);
#5966=ORIENTED_EDGE('',*,*,#4461,.F.);
#5967=ORIENTED_EDGE('',*,*,#4458,.F.);
#5968=ORIENTED_EDGE('',*,*,#4455,.F.);
#5969=ORIENTED_EDGE('',*,*,#4452,.F.);
#5970=ORIENTED_EDGE('',*,*,#4449,.F.);
#5971=ORIENTED_EDGE('',*,*,#4446,.F.);
#5972=ORIENTED_EDGE('',*,*,#4443,.F.);
#5973=ORIENTED_EDGE('',*,*,#4440,.F.);
#5974=ORIENTED_EDGE('',*,*,#4543,.F.);
#5975=ORIENTED_EDGE('',*,*,#4435,.F.);
#5976=ORIENTED_EDGE('',*,*,#4442,.F.);
#5977=ORIENTED_EDGE('',*,*,#4445,.F.);
#5978=ORIENTED_EDGE('',*,*,#4448,.F.);
#5979=ORIENTED_EDGE('',*,*,#4451,.F.);
#5980=ORIENTED_EDGE('',*,*,#4454,.F.);
#5981=ORIENTED_EDGE('',*,*,#4457,.F.);
#5982=ORIENTED_EDGE('',*,*,#4460,.F.);
#5983=ORIENTED_EDGE('',*,*,#4463,.F.);
#5984=ORIENTED_EDGE('',*,*,#4466,.F.);
#5985=ORIENTED_EDGE('',*,*,#4469,.F.);
#5986=ORIENTED_EDGE('',*,*,#4472,.F.);
#5987=ORIENTED_EDGE('',*,*,#4475,.F.);
#5988=ORIENTED_EDGE('',*,*,#4478,.F.);
#5989=ORIENTED_EDGE('',*,*,#4481,.F.);
#5990=ORIENTED_EDGE('',*,*,#4484,.F.);
#5991=ORIENTED_EDGE('',*,*,#4549,.F.);
#5992=ORIENTED_EDGE('',*,*,#4489,.F.);
#5993=ORIENTED_EDGE('',*,*,#4550,.F.);
#5994=ORIENTED_EDGE('',*,*,#4540,.T.);
#5995=ORIENTED_EDGE('',*,*,#4546,.T.);
#5996=ORIENTED_EDGE('',*,*,#4538,.T.);
#5997=ORIENTED_EDGE('',*,*,#4535,.T.);
#5998=ORIENTED_EDGE('',*,*,#4532,.T.);
#5999=ORIENTED_EDGE('',*,*,#4529,.T.);
#6000=ORIENTED_EDGE('',*,*,#4526,.T.);
#6001=ORIENTED_EDGE('',*,*,#4523,.T.);
#6002=ORIENTED_EDGE('',*,*,#4520,.T.);
#6003=ORIENTED_EDGE('',*,*,#4517,.T.);
#6004=ORIENTED_EDGE('',*,*,#4514,.T.);
#6005=ORIENTED_EDGE('',*,*,#4511,.T.);
#6006=ORIENTED_EDGE('',*,*,#4508,.T.);
#6007=ORIENTED_EDGE('',*,*,#4505,.T.);
#6008=ORIENTED_EDGE('',*,*,#4502,.T.);
#6009=ORIENTED_EDGE('',*,*,#4499,.T.);
#6010=ORIENTED_EDGE('',*,*,#4496,.T.);
#6011=ORIENTED_EDGE('',*,*,#4493,.T.);
#6012=ORIENTED_EDGE('',*,*,#4486,.T.);
#6013=ORIENTED_EDGE('',*,*,#4549,.T.);
#6014=ORIENTED_EDGE('',*,*,#4483,.F.);
#6015=ORIENTED_EDGE('',*,*,#4548,.T.);
#6016=ORIENTED_EDGE('',*,*,#4327,.F.);
#6017=ORIENTED_EDGE('',*,*,#4551,.T.);
#6018=ORIENTED_EDGE('',*,*,#4383,.T.);
#6019=ORIENTED_EDGE('',*,*,#4552,.T.);
#6020=ORIENTED_EDGE('',*,*,#4330,.F.);
#6021=ORIENTED_EDGE('',*,*,#4430,.T.);
#6022=ORIENTED_EDGE('',*,*,#4553,.T.);
#6023=ORIENTED_EDGE('',*,*,#4427,.F.);
#6024=ORIENTED_EDGE('',*,*,#4554,.F.);
#6025=ORIENTED_EDGE('',*,*,#4552,.F.);
#6026=ORIENTED_EDGE('',*,*,#4382,.F.);
#6027=ORIENTED_EDGE('',*,*,#4386,.F.);
#6028=ORIENTED_EDGE('',*,*,#4389,.F.);
#6029=ORIENTED_EDGE('',*,*,#4392,.F.);
#6030=ORIENTED_EDGE('',*,*,#4395,.F.);
#6031=ORIENTED_EDGE('',*,*,#4398,.F.);
#6032=ORIENTED_EDGE('',*,*,#4401,.F.);
#6033=ORIENTED_EDGE('',*,*,#4404,.F.);
#6034=ORIENTED_EDGE('',*,*,#4407,.F.);
#6035=ORIENTED_EDGE('',*,*,#4410,.F.);
#6036=ORIENTED_EDGE('',*,*,#4413,.F.);
#6037=ORIENTED_EDGE('',*,*,#4416,.F.);
#6038=ORIENTED_EDGE('',*,*,#4419,.F.);
#6039=ORIENTED_EDGE('',*,*,#4422,.F.);
#6040=ORIENTED_EDGE('',*,*,#4425,.F.);
#6041=ORIENTED_EDGE('',*,*,#4428,.F.);
#6042=ORIENTED_EDGE('',*,*,#4553,.F.);
#6043=ORIENTED_EDGE('',*,*,#4433,.F.);
#6044=ORIENTED_EDGE('',*,*,#4555,.F.);
#6045=ORIENTED_EDGE('',*,*,#4378,.F.);
#6046=ORIENTED_EDGE('',*,*,#4556,.F.);
#6047=ORIENTED_EDGE('',*,*,#4376,.F.);
#6048=ORIENTED_EDGE('',*,*,#4373,.F.);
#6049=ORIENTED_EDGE('',*,*,#4370,.F.);
#6050=ORIENTED_EDGE('',*,*,#4367,.F.);
#6051=ORIENTED_EDGE('',*,*,#4364,.F.);
#6052=ORIENTED_EDGE('',*,*,#4361,.F.);
#6053=ORIENTED_EDGE('',*,*,#4358,.F.);
#6054=ORIENTED_EDGE('',*,*,#4355,.F.);
#6055=ORIENTED_EDGE('',*,*,#4352,.F.);
#6056=ORIENTED_EDGE('',*,*,#4349,.F.);
#6057=ORIENTED_EDGE('',*,*,#4346,.F.);
#6058=ORIENTED_EDGE('',*,*,#4343,.F.);
#6059=ORIENTED_EDGE('',*,*,#4340,.F.);
#6060=ORIENTED_EDGE('',*,*,#4337,.F.);
#6061=ORIENTED_EDGE('',*,*,#4334,.F.);
#6062=ORIENTED_EDGE('',*,*,#4331,.F.);
#6063=ORIENTED_EDGE('',*,*,#4551,.F.);
#6064=ORIENTED_EDGE('',*,*,#4326,.F.);
#6065=ORIENTED_EDGE('',*,*,#4333,.F.);
#6066=ORIENTED_EDGE('',*,*,#4336,.F.);
#6067=ORIENTED_EDGE('',*,*,#4339,.F.);
#6068=ORIENTED_EDGE('',*,*,#4342,.F.);
#6069=ORIENTED_EDGE('',*,*,#4345,.F.);
#6070=ORIENTED_EDGE('',*,*,#4348,.F.);
#6071=ORIENTED_EDGE('',*,*,#4351,.F.);
#6072=ORIENTED_EDGE('',*,*,#4354,.F.);
#6073=ORIENTED_EDGE('',*,*,#4357,.F.);
#6074=ORIENTED_EDGE('',*,*,#4360,.F.);
#6075=ORIENTED_EDGE('',*,*,#4363,.F.);
#6076=ORIENTED_EDGE('',*,*,#4366,.F.);
#6077=ORIENTED_EDGE('',*,*,#4369,.F.);
#6078=ORIENTED_EDGE('',*,*,#4372,.F.);
#6079=ORIENTED_EDGE('',*,*,#4375,.F.);
#6080=ORIENTED_EDGE('',*,*,#4557,.F.);
#6081=ORIENTED_EDGE('',*,*,#4380,.F.);
#6082=ORIENTED_EDGE('',*,*,#4558,.F.);
#6083=ORIENTED_EDGE('',*,*,#4431,.T.);
#6084=ORIENTED_EDGE('',*,*,#4554,.T.);
#6085=ORIENTED_EDGE('',*,*,#4429,.T.);
#6086=ORIENTED_EDGE('',*,*,#4426,.T.);
#6087=ORIENTED_EDGE('',*,*,#4423,.T.);
#6088=ORIENTED_EDGE('',*,*,#4420,.T.);
#6089=ORIENTED_EDGE('',*,*,#4417,.T.);
#6090=ORIENTED_EDGE('',*,*,#4414,.T.);
#6091=ORIENTED_EDGE('',*,*,#4411,.T.);
#6092=ORIENTED_EDGE('',*,*,#4408,.T.);
#6093=ORIENTED_EDGE('',*,*,#4405,.T.);
#6094=ORIENTED_EDGE('',*,*,#4402,.T.);
#6095=ORIENTED_EDGE('',*,*,#4399,.T.);
#6096=ORIENTED_EDGE('',*,*,#4396,.T.);
#6097=ORIENTED_EDGE('',*,*,#4393,.T.);
#6098=ORIENTED_EDGE('',*,*,#4390,.T.);
#6099=ORIENTED_EDGE('',*,*,#4387,.T.);
#6100=ORIENTED_EDGE('',*,*,#4384,.T.);
#6101=ORIENTED_EDGE('',*,*,#4377,.T.);
#6102=ORIENTED_EDGE('',*,*,#4557,.T.);
#6103=ORIENTED_EDGE('',*,*,#4374,.F.);
#6104=ORIENTED_EDGE('',*,*,#4556,.T.);
#6105=ORIENTED_EDGE('',*,*,#4218,.F.);
#6106=ORIENTED_EDGE('',*,*,#4559,.T.);
#6107=ORIENTED_EDGE('',*,*,#4274,.T.);
#6108=ORIENTED_EDGE('',*,*,#4560,.T.);
#6109=ORIENTED_EDGE('',*,*,#4221,.F.);
#6110=ORIENTED_EDGE('',*,*,#4321,.T.);
#6111=ORIENTED_EDGE('',*,*,#4561,.T.);
#6112=ORIENTED_EDGE('',*,*,#4318,.F.);
#6113=ORIENTED_EDGE('',*,*,#4562,.F.);
#6114=ORIENTED_EDGE('',*,*,#4560,.F.);
#6115=ORIENTED_EDGE('',*,*,#4273,.F.);
#6116=ORIENTED_EDGE('',*,*,#4277,.F.);
#6117=ORIENTED_EDGE('',*,*,#4280,.F.);
#6118=ORIENTED_EDGE('',*,*,#4283,.F.);
#6119=ORIENTED_EDGE('',*,*,#4286,.F.);
#6120=ORIENTED_EDGE('',*,*,#4289,.F.);
#6121=ORIENTED_EDGE('',*,*,#4292,.F.);
#6122=ORIENTED_EDGE('',*,*,#4295,.F.);
#6123=ORIENTED_EDGE('',*,*,#4298,.F.);
#6124=ORIENTED_EDGE('',*,*,#4301,.F.);
#6125=ORIENTED_EDGE('',*,*,#4304,.F.);
#6126=ORIENTED_EDGE('',*,*,#4307,.F.);
#6127=ORIENTED_EDGE('',*,*,#4310,.F.);
#6128=ORIENTED_EDGE('',*,*,#4313,.F.);
#6129=ORIENTED_EDGE('',*,*,#4316,.F.);
#6130=ORIENTED_EDGE('',*,*,#4319,.F.);
#6131=ORIENTED_EDGE('',*,*,#4561,.F.);
#6132=ORIENTED_EDGE('',*,*,#4324,.F.);
#6133=ORIENTED_EDGE('',*,*,#4563,.F.);
#6134=ORIENTED_EDGE('',*,*,#4269,.F.);
#6135=ORIENTED_EDGE('',*,*,#4564,.F.);
#6136=ORIENTED_EDGE('',*,*,#4267,.F.);
#6137=ORIENTED_EDGE('',*,*,#4264,.F.);
#6138=ORIENTED_EDGE('',*,*,#4261,.F.);
#6139=ORIENTED_EDGE('',*,*,#4258,.F.);
#6140=ORIENTED_EDGE('',*,*,#4255,.F.);
#6141=ORIENTED_EDGE('',*,*,#4252,.F.);
#6142=ORIENTED_EDGE('',*,*,#4249,.F.);
#6143=ORIENTED_EDGE('',*,*,#4246,.F.);
#6144=ORIENTED_EDGE('',*,*,#4243,.F.);
#6145=ORIENTED_EDGE('',*,*,#4240,.F.);
#6146=ORIENTED_EDGE('',*,*,#4237,.F.);
#6147=ORIENTED_EDGE('',*,*,#4234,.F.);
#6148=ORIENTED_EDGE('',*,*,#4231,.F.);
#6149=ORIENTED_EDGE('',*,*,#4228,.F.);
#6150=ORIENTED_EDGE('',*,*,#4225,.F.);
#6151=ORIENTED_EDGE('',*,*,#4222,.F.);
#6152=ORIENTED_EDGE('',*,*,#4559,.F.);
#6153=ORIENTED_EDGE('',*,*,#4217,.F.);
#6154=ORIENTED_EDGE('',*,*,#4224,.F.);
#6155=ORIENTED_EDGE('',*,*,#4227,.F.);
#6156=ORIENTED_EDGE('',*,*,#4230,.F.);
#6157=ORIENTED_EDGE('',*,*,#4233,.F.);
#6158=ORIENTED_EDGE('',*,*,#4236,.F.);
#6159=ORIENTED_EDGE('',*,*,#4239,.F.);
#6160=ORIENTED_EDGE('',*,*,#4242,.F.);
#6161=ORIENTED_EDGE('',*,*,#4245,.F.);
#6162=ORIENTED_EDGE('',*,*,#4248,.F.);
#6163=ORIENTED_EDGE('',*,*,#4251,.F.);
#6164=ORIENTED_EDGE('',*,*,#4254,.F.);
#6165=ORIENTED_EDGE('',*,*,#4257,.F.);
#6166=ORIENTED_EDGE('',*,*,#4260,.F.);
#6167=ORIENTED_EDGE('',*,*,#4263,.F.);
#6168=ORIENTED_EDGE('',*,*,#4266,.F.);
#6169=ORIENTED_EDGE('',*,*,#4565,.F.);
#6170=ORIENTED_EDGE('',*,*,#4271,.F.);
#6171=ORIENTED_EDGE('',*,*,#4566,.F.);
#6172=ORIENTED_EDGE('',*,*,#4322,.T.);
#6173=ORIENTED_EDGE('',*,*,#4562,.T.);
#6174=ORIENTED_EDGE('',*,*,#4320,.T.);
#6175=ORIENTED_EDGE('',*,*,#4317,.T.);
#6176=ORIENTED_EDGE('',*,*,#4314,.T.);
#6177=ORIENTED_EDGE('',*,*,#4311,.T.);
#6178=ORIENTED_EDGE('',*,*,#4308,.T.);
#6179=ORIENTED_EDGE('',*,*,#4305,.T.);
#6180=ORIENTED_EDGE('',*,*,#4302,.T.);
#6181=ORIENTED_EDGE('',*,*,#4299,.T.);
#6182=ORIENTED_EDGE('',*,*,#4296,.T.);
#6183=ORIENTED_EDGE('',*,*,#4293,.T.);
#6184=ORIENTED_EDGE('',*,*,#4290,.T.);
#6185=ORIENTED_EDGE('',*,*,#4287,.T.);
#6186=ORIENTED_EDGE('',*,*,#4284,.T.);
#6187=ORIENTED_EDGE('',*,*,#4281,.T.);
#6188=ORIENTED_EDGE('',*,*,#4278,.T.);
#6189=ORIENTED_EDGE('',*,*,#4275,.T.);
#6190=ORIENTED_EDGE('',*,*,#4268,.T.);
#6191=ORIENTED_EDGE('',*,*,#4565,.T.);
#6192=ORIENTED_EDGE('',*,*,#4265,.F.);
#6193=ORIENTED_EDGE('',*,*,#4564,.T.);
#6194=ORIENTED_EDGE('',*,*,#4109,.F.);
#6195=ORIENTED_EDGE('',*,*,#4567,.T.);
#6196=ORIENTED_EDGE('',*,*,#4165,.T.);
#6197=ORIENTED_EDGE('',*,*,#4568,.T.);
#6198=ORIENTED_EDGE('',*,*,#4112,.F.);
#6199=ORIENTED_EDGE('',*,*,#4212,.T.);
#6200=ORIENTED_EDGE('',*,*,#4569,.T.);
#6201=ORIENTED_EDGE('',*,*,#4209,.F.);
#6202=ORIENTED_EDGE('',*,*,#4570,.F.);
#6203=ORIENTED_EDGE('',*,*,#4568,.F.);
#6204=ORIENTED_EDGE('',*,*,#4164,.F.);
#6205=ORIENTED_EDGE('',*,*,#4168,.F.);
#6206=ORIENTED_EDGE('',*,*,#4171,.F.);
#6207=ORIENTED_EDGE('',*,*,#4174,.F.);
#6208=ORIENTED_EDGE('',*,*,#4177,.F.);
#6209=ORIENTED_EDGE('',*,*,#4180,.F.);
#6210=ORIENTED_EDGE('',*,*,#4183,.F.);
#6211=ORIENTED_EDGE('',*,*,#4186,.F.);
#6212=ORIENTED_EDGE('',*,*,#4189,.F.);
#6213=ORIENTED_EDGE('',*,*,#4192,.F.);
#6214=ORIENTED_EDGE('',*,*,#4195,.F.);
#6215=ORIENTED_EDGE('',*,*,#4198,.F.);
#6216=ORIENTED_EDGE('',*,*,#4201,.F.);
#6217=ORIENTED_EDGE('',*,*,#4204,.F.);
#6218=ORIENTED_EDGE('',*,*,#4207,.F.);
#6219=ORIENTED_EDGE('',*,*,#4210,.F.);
#6220=ORIENTED_EDGE('',*,*,#4569,.F.);
#6221=ORIENTED_EDGE('',*,*,#4215,.F.);
#6222=ORIENTED_EDGE('',*,*,#4571,.F.);
#6223=ORIENTED_EDGE('',*,*,#4160,.F.);
#6224=ORIENTED_EDGE('',*,*,#4572,.F.);
#6225=ORIENTED_EDGE('',*,*,#4158,.F.);
#6226=ORIENTED_EDGE('',*,*,#4155,.F.);
#6227=ORIENTED_EDGE('',*,*,#4152,.F.);
#6228=ORIENTED_EDGE('',*,*,#4149,.F.);
#6229=ORIENTED_EDGE('',*,*,#4146,.F.);
#6230=ORIENTED_EDGE('',*,*,#4143,.F.);
#6231=ORIENTED_EDGE('',*,*,#4140,.F.);
#6232=ORIENTED_EDGE('',*,*,#4137,.F.);
#6233=ORIENTED_EDGE('',*,*,#4134,.F.);
#6234=ORIENTED_EDGE('',*,*,#4131,.F.);
#6235=ORIENTED_EDGE('',*,*,#4128,.F.);
#6236=ORIENTED_EDGE('',*,*,#4125,.F.);
#6237=ORIENTED_EDGE('',*,*,#4122,.F.);
#6238=ORIENTED_EDGE('',*,*,#4119,.F.);
#6239=ORIENTED_EDGE('',*,*,#4116,.F.);
#6240=ORIENTED_EDGE('',*,*,#4113,.F.);
#6241=ORIENTED_EDGE('',*,*,#4567,.F.);
#6242=ORIENTED_EDGE('',*,*,#4108,.F.);
#6243=ORIENTED_EDGE('',*,*,#4115,.F.);
#6244=ORIENTED_EDGE('',*,*,#4118,.F.);
#6245=ORIENTED_EDGE('',*,*,#4121,.F.);
#6246=ORIENTED_EDGE('',*,*,#4124,.F.);
#6247=ORIENTED_EDGE('',*,*,#4127,.F.);
#6248=ORIENTED_EDGE('',*,*,#4130,.F.);
#6249=ORIENTED_EDGE('',*,*,#4133,.F.);
#6250=ORIENTED_EDGE('',*,*,#4136,.F.);
#6251=ORIENTED_EDGE('',*,*,#4139,.F.);
#6252=ORIENTED_EDGE('',*,*,#4142,.F.);
#6253=ORIENTED_EDGE('',*,*,#4145,.F.);
#6254=ORIENTED_EDGE('',*,*,#4148,.F.);
#6255=ORIENTED_EDGE('',*,*,#4151,.F.);
#6256=ORIENTED_EDGE('',*,*,#4154,.F.);
#6257=ORIENTED_EDGE('',*,*,#4157,.F.);
#6258=ORIENTED_EDGE('',*,*,#4573,.F.);
#6259=ORIENTED_EDGE('',*,*,#4162,.F.);
#6260=ORIENTED_EDGE('',*,*,#4574,.F.);
#6261=ORIENTED_EDGE('',*,*,#4213,.T.);
#6262=ORIENTED_EDGE('',*,*,#4570,.T.);
#6263=ORIENTED_EDGE('',*,*,#4211,.T.);
#6264=ORIENTED_EDGE('',*,*,#4208,.T.);
#6265=ORIENTED_EDGE('',*,*,#4205,.T.);
#6266=ORIENTED_EDGE('',*,*,#4202,.T.);
#6267=ORIENTED_EDGE('',*,*,#4199,.T.);
#6268=ORIENTED_EDGE('',*,*,#4196,.T.);
#6269=ORIENTED_EDGE('',*,*,#4193,.T.);
#6270=ORIENTED_EDGE('',*,*,#4190,.T.);
#6271=ORIENTED_EDGE('',*,*,#4187,.T.);
#6272=ORIENTED_EDGE('',*,*,#4184,.T.);
#6273=ORIENTED_EDGE('',*,*,#4181,.T.);
#6274=ORIENTED_EDGE('',*,*,#4178,.T.);
#6275=ORIENTED_EDGE('',*,*,#4175,.T.);
#6276=ORIENTED_EDGE('',*,*,#4172,.T.);
#6277=ORIENTED_EDGE('',*,*,#4169,.T.);
#6278=ORIENTED_EDGE('',*,*,#4166,.T.);
#6279=ORIENTED_EDGE('',*,*,#4159,.T.);
#6280=ORIENTED_EDGE('',*,*,#4573,.T.);
#6281=ORIENTED_EDGE('',*,*,#4156,.F.);
#6282=ORIENTED_EDGE('',*,*,#4572,.T.);
#6283=ORIENTED_EDGE('',*,*,#4329,.F.);
#6284=ORIENTED_EDGE('',*,*,#4220,.F.);
#6285=ORIENTED_EDGE('',*,*,#4438,.F.);
#6286=ORIENTED_EDGE('',*,*,#4111,.F.);
#6287=ORIENTED_EDGE('',*,*,#4575,.T.);
#6288=ORIENTED_EDGE('',*,*,#4576,.T.);
#6289=ORIENTED_EDGE('',*,*,#4577,.F.);
#6290=ORIENTED_EDGE('',*,*,#4578,.F.);
#6291=ORIENTED_EDGE('',*,*,#4579,.T.);
#6292=ORIENTED_EDGE('',*,*,#4578,.T.);
#6293=ORIENTED_EDGE('',*,*,#4580,.F.);
#6294=ORIENTED_EDGE('',*,*,#4581,.F.);
#6295=ORIENTED_EDGE('',*,*,#4582,.T.);
#6296=ORIENTED_EDGE('',*,*,#4581,.T.);
#6297=ORIENTED_EDGE('',*,*,#4583,.F.);
#6298=ORIENTED_EDGE('',*,*,#4584,.F.);
#6299=ORIENTED_EDGE('',*,*,#4585,.T.);
#6300=ORIENTED_EDGE('',*,*,#4584,.T.);
#6301=ORIENTED_EDGE('',*,*,#4586,.F.);
#6302=ORIENTED_EDGE('',*,*,#4576,.F.);
#6303=ORIENTED_EDGE('',*,*,#4587,.T.);
#6304=ORIENTED_EDGE('',*,*,#4588,.T.);
#6305=ORIENTED_EDGE('',*,*,#4589,.F.);
#6306=ORIENTED_EDGE('',*,*,#4590,.F.);
#6307=ORIENTED_EDGE('',*,*,#4591,.T.);
#6308=ORIENTED_EDGE('',*,*,#4590,.T.);
#6309=ORIENTED_EDGE('',*,*,#4592,.F.);
#6310=ORIENTED_EDGE('',*,*,#4593,.F.);
#6311=ORIENTED_EDGE('',*,*,#4594,.T.);
#6312=ORIENTED_EDGE('',*,*,#4593,.T.);
#6313=ORIENTED_EDGE('',*,*,#4595,.F.);
#6314=ORIENTED_EDGE('',*,*,#4596,.F.);
#6315=ORIENTED_EDGE('',*,*,#4597,.T.);
#6316=ORIENTED_EDGE('',*,*,#4596,.T.);
#6317=ORIENTED_EDGE('',*,*,#4598,.F.);
#6318=ORIENTED_EDGE('',*,*,#4588,.F.);
#6319=ORIENTED_EDGE('',*,*,#4598,.T.);
#6320=ORIENTED_EDGE('',*,*,#4595,.T.);
#6321=ORIENTED_EDGE('',*,*,#4592,.T.);
#6322=ORIENTED_EDGE('',*,*,#4589,.T.);
#6323=ORIENTED_EDGE('',*,*,#4586,.T.);
#6324=ORIENTED_EDGE('',*,*,#4583,.T.);
#6325=ORIENTED_EDGE('',*,*,#4580,.T.);
#6326=ORIENTED_EDGE('',*,*,#4577,.T.);
#6327=ORIENTED_EDGE('',*,*,#4597,.F.);
#6328=ORIENTED_EDGE('',*,*,#4587,.F.);
#6329=ORIENTED_EDGE('',*,*,#4591,.F.);
#6330=ORIENTED_EDGE('',*,*,#4594,.F.);
#6331=ORIENTED_EDGE('',*,*,#4550,.T.);
#6332=ORIENTED_EDGE('',*,*,#4488,.T.);
#6333=ORIENTED_EDGE('',*,*,#4547,.T.);
#6334=ORIENTED_EDGE('',*,*,#4541,.T.);
#6335=ORIENTED_EDGE('',*,*,#4558,.T.);
#6336=ORIENTED_EDGE('',*,*,#4379,.T.);
#6337=ORIENTED_EDGE('',*,*,#4555,.T.);
#6338=ORIENTED_EDGE('',*,*,#4432,.T.);
#6339=ORIENTED_EDGE('',*,*,#4566,.T.);
#6340=ORIENTED_EDGE('',*,*,#4270,.T.);
#6341=ORIENTED_EDGE('',*,*,#4563,.T.);
#6342=ORIENTED_EDGE('',*,*,#4323,.T.);
#6343=ORIENTED_EDGE('',*,*,#4574,.T.);
#6344=ORIENTED_EDGE('',*,*,#4161,.T.);
#6345=ORIENTED_EDGE('',*,*,#4571,.T.);
#6346=ORIENTED_EDGE('',*,*,#4214,.T.);
#6347=ORIENTED_EDGE('',*,*,#4585,.F.);
#6348=ORIENTED_EDGE('',*,*,#4575,.F.);
#6349=ORIENTED_EDGE('',*,*,#4579,.F.);
#6350=ORIENTED_EDGE('',*,*,#4582,.F.);
#6351=ORIENTED_EDGE('',*,*,#4599,.F.);
#6352=ORIENTED_EDGE('',*,*,#4600,.T.);
#6353=ORIENTED_EDGE('',*,*,#4601,.F.);
#6354=ORIENTED_EDGE('',*,*,#4600,.F.);
#6355=ORIENTED_EDGE('',*,*,#4602,.F.);
#6356=ORIENTED_EDGE('',*,*,#4603,.T.);
#6357=ORIENTED_EDGE('',*,*,#4604,.F.);
#6358=ORIENTED_EDGE('',*,*,#4603,.F.);
#6359=ORIENTED_EDGE('',*,*,#4605,.F.);
#6360=ORIENTED_EDGE('',*,*,#4606,.T.);
#6361=ORIENTED_EDGE('',*,*,#4607,.F.);
#6362=ORIENTED_EDGE('',*,*,#4606,.F.);
#6363=ORIENTED_EDGE('',*,*,#4608,.F.);
#6364=ORIENTED_EDGE('',*,*,#4609,.T.);
#6365=ORIENTED_EDGE('',*,*,#4610,.F.);
#6366=ORIENTED_EDGE('',*,*,#4609,.F.);
#6367=ORIENTED_EDGE('',*,*,#4611,.F.);
#6368=ORIENTED_EDGE('',*,*,#4612,.T.);
#6369=ORIENTED_EDGE('',*,*,#4613,.F.);
#6370=ORIENTED_EDGE('',*,*,#4612,.F.);
#6371=ORIENTED_EDGE('',*,*,#4614,.T.);
#6372=ORIENTED_EDGE('',*,*,#4615,.T.);
#6373=ORIENTED_EDGE('',*,*,#4616,.F.);
#6374=ORIENTED_EDGE('',*,*,#4617,.F.);
#6375=ORIENTED_EDGE('',*,*,#4618,.T.);
#6376=ORIENTED_EDGE('',*,*,#4617,.T.);
#6377=ORIENTED_EDGE('',*,*,#4619,.F.);
#6378=ORIENTED_EDGE('',*,*,#4620,.F.);
#6379=ORIENTED_EDGE('',*,*,#4621,.T.);
#6380=ORIENTED_EDGE('',*,*,#4620,.T.);
#6381=ORIENTED_EDGE('',*,*,#4622,.F.);
#6382=ORIENTED_EDGE('',*,*,#4623,.F.);
#6383=ORIENTED_EDGE('',*,*,#4624,.T.);
#6384=ORIENTED_EDGE('',*,*,#4623,.T.);
#6385=ORIENTED_EDGE('',*,*,#4625,.F.);
#6386=ORIENTED_EDGE('',*,*,#4615,.F.);
#6387=ORIENTED_EDGE('',*,*,#4625,.T.);
#6388=ORIENTED_EDGE('',*,*,#4622,.T.);
#6389=ORIENTED_EDGE('',*,*,#4619,.T.);
#6390=ORIENTED_EDGE('',*,*,#4616,.T.);
#6391=ORIENTED_EDGE('',*,*,#4599,.T.);
#6392=ORIENTED_EDGE('',*,*,#4602,.T.);
#6393=ORIENTED_EDGE('',*,*,#4605,.T.);
#6394=ORIENTED_EDGE('',*,*,#4608,.T.);
#6395=ORIENTED_EDGE('',*,*,#4611,.T.);
#6396=ORIENTED_EDGE('',*,*,#4624,.F.);
#6397=ORIENTED_EDGE('',*,*,#4614,.F.);
#6398=ORIENTED_EDGE('',*,*,#4618,.F.);
#6399=ORIENTED_EDGE('',*,*,#4621,.F.);
#6400=ORIENTED_EDGE('',*,*,#4601,.T.);
#6401=ORIENTED_EDGE('',*,*,#4604,.T.);
#6402=ORIENTED_EDGE('',*,*,#4607,.T.);
#6403=ORIENTED_EDGE('',*,*,#4610,.T.);
#6404=ORIENTED_EDGE('',*,*,#4613,.T.);
#6405=ORIENTED_EDGE('',*,*,#4626,.T.);
#6406=ORIENTED_EDGE('',*,*,#4627,.T.);
#6407=ORIENTED_EDGE('',*,*,#4628,.F.);
#6408=ORIENTED_EDGE('',*,*,#4629,.F.);
#6409=ORIENTED_EDGE('',*,*,#4630,.T.);
#6410=ORIENTED_EDGE('',*,*,#4629,.T.);
#6411=ORIENTED_EDGE('',*,*,#4631,.F.);
#6412=ORIENTED_EDGE('',*,*,#4632,.F.);
#6413=ORIENTED_EDGE('',*,*,#4633,.T.);
#6414=ORIENTED_EDGE('',*,*,#4632,.T.);
#6415=ORIENTED_EDGE('',*,*,#4634,.F.);
#6416=ORIENTED_EDGE('',*,*,#4635,.F.);
#6417=ORIENTED_EDGE('',*,*,#4636,.T.);
#6418=ORIENTED_EDGE('',*,*,#4635,.T.);
#6419=ORIENTED_EDGE('',*,*,#4637,.F.);
#6420=ORIENTED_EDGE('',*,*,#4627,.F.);
#6421=ORIENTED_EDGE('',*,*,#4638,.T.);
#6422=ORIENTED_EDGE('',*,*,#4639,.T.);
#6423=ORIENTED_EDGE('',*,*,#4640,.F.);
#6424=ORIENTED_EDGE('',*,*,#4641,.F.);
#6425=ORIENTED_EDGE('',*,*,#4642,.T.);
#6426=ORIENTED_EDGE('',*,*,#4641,.T.);
#6427=ORIENTED_EDGE('',*,*,#4643,.F.);
#6428=ORIENTED_EDGE('',*,*,#4644,.F.);
#6429=ORIENTED_EDGE('',*,*,#4645,.T.);
#6430=ORIENTED_EDGE('',*,*,#4644,.T.);
#6431=ORIENTED_EDGE('',*,*,#4646,.F.);
#6432=ORIENTED_EDGE('',*,*,#4647,.F.);
#6433=ORIENTED_EDGE('',*,*,#4648,.T.);
#6434=ORIENTED_EDGE('',*,*,#4647,.T.);
#6435=ORIENTED_EDGE('',*,*,#4649,.F.);
#6436=ORIENTED_EDGE('',*,*,#4639,.F.);
#6437=ORIENTED_EDGE('',*,*,#4649,.T.);
#6438=ORIENTED_EDGE('',*,*,#4646,.T.);
#6439=ORIENTED_EDGE('',*,*,#4643,.T.);
#6440=ORIENTED_EDGE('',*,*,#4640,.T.);
#6441=ORIENTED_EDGE('',*,*,#4637,.T.);
#6442=ORIENTED_EDGE('',*,*,#4634,.T.);
#6443=ORIENTED_EDGE('',*,*,#4631,.T.);
#6444=ORIENTED_EDGE('',*,*,#4628,.T.);
#6445=ORIENTED_EDGE('',*,*,#4648,.F.);
#6446=ORIENTED_EDGE('',*,*,#4638,.F.);
#6447=ORIENTED_EDGE('',*,*,#4642,.F.);
#6448=ORIENTED_EDGE('',*,*,#4645,.F.);
#6449=ORIENTED_EDGE('',*,*,#4636,.F.);
#6450=ORIENTED_EDGE('',*,*,#4626,.F.);
#6451=ORIENTED_EDGE('',*,*,#4630,.F.);
#6452=ORIENTED_EDGE('',*,*,#4633,.F.);
#6453=ORIENTED_EDGE('',*,*,#4650,.T.);
#6454=ORIENTED_EDGE('',*,*,#4651,.T.);
#6455=ORIENTED_EDGE('',*,*,#4652,.T.);
#6456=ORIENTED_EDGE('',*,*,#4653,.T.);
#6457=ORIENTED_EDGE('',*,*,#4654,.T.);
#6458=ORIENTED_EDGE('',*,*,#4655,.T.);
#6459=ORIENTED_EDGE('',*,*,#4654,.F.);
#6460=ORIENTED_EDGE('',*,*,#4656,.T.);
#6461=ORIENTED_EDGE('',*,*,#4657,.T.);
#6462=ORIENTED_EDGE('',*,*,#4658,.T.);
#6463=ORIENTED_EDGE('',*,*,#4650,.F.);
#6464=ORIENTED_EDGE('',*,*,#4659,.T.);
#6465=ORIENTED_EDGE('',*,*,#4660,.T.);
#6466=ORIENTED_EDGE('',*,*,#4661,.T.);
#6467=ORIENTED_EDGE('',*,*,#4657,.F.);
#6468=ORIENTED_EDGE('',*,*,#4662,.T.);
#6469=ORIENTED_EDGE('',*,*,#4663,.T.);
#6470=ORIENTED_EDGE('',*,*,#4664,.T.);
#6471=ORIENTED_EDGE('',*,*,#4660,.F.);
#6472=ORIENTED_EDGE('',*,*,#4665,.T.);
#6473=ORIENTED_EDGE('',*,*,#4666,.T.);
#6474=ORIENTED_EDGE('',*,*,#4667,.T.);
#6475=ORIENTED_EDGE('',*,*,#4663,.F.);
#6476=ORIENTED_EDGE('',*,*,#4668,.T.);
#6477=ORIENTED_EDGE('',*,*,#4669,.T.);
#6478=ORIENTED_EDGE('',*,*,#4670,.T.);
#6479=ORIENTED_EDGE('',*,*,#4666,.F.);
#6480=ORIENTED_EDGE('',*,*,#4671,.T.);
#6481=ORIENTED_EDGE('',*,*,#4672,.T.);
#6482=ORIENTED_EDGE('',*,*,#4673,.T.);
#6483=ORIENTED_EDGE('',*,*,#4669,.F.);
#6484=ORIENTED_EDGE('',*,*,#4674,.T.);
#6485=ORIENTED_EDGE('',*,*,#4675,.T.);
#6486=ORIENTED_EDGE('',*,*,#4676,.T.);
#6487=ORIENTED_EDGE('',*,*,#4672,.F.);
#6488=ORIENTED_EDGE('',*,*,#4677,.T.);
#6489=ORIENTED_EDGE('',*,*,#4678,.T.);
#6490=ORIENTED_EDGE('',*,*,#4679,.T.);
#6491=ORIENTED_EDGE('',*,*,#4675,.F.);
#6492=ORIENTED_EDGE('',*,*,#4680,.T.);
#6493=ORIENTED_EDGE('',*,*,#4681,.T.);
#6494=ORIENTED_EDGE('',*,*,#4682,.T.);
#6495=ORIENTED_EDGE('',*,*,#4678,.F.);
#6496=ORIENTED_EDGE('',*,*,#4683,.T.);
#6497=ORIENTED_EDGE('',*,*,#4684,.T.);
#6498=ORIENTED_EDGE('',*,*,#4685,.T.);
#6499=ORIENTED_EDGE('',*,*,#4681,.F.);
#6500=ORIENTED_EDGE('',*,*,#4686,.T.);
#6501=ORIENTED_EDGE('',*,*,#4687,.T.);
#6502=ORIENTED_EDGE('',*,*,#4688,.T.);
#6503=ORIENTED_EDGE('',*,*,#4684,.F.);
#6504=ORIENTED_EDGE('',*,*,#4689,.T.);
#6505=ORIENTED_EDGE('',*,*,#4690,.T.);
#6506=ORIENTED_EDGE('',*,*,#4691,.T.);
#6507=ORIENTED_EDGE('',*,*,#4687,.F.);
#6508=ORIENTED_EDGE('',*,*,#4692,.T.);
#6509=ORIENTED_EDGE('',*,*,#4693,.T.);
#6510=ORIENTED_EDGE('',*,*,#4694,.T.);
#6511=ORIENTED_EDGE('',*,*,#4690,.F.);
#6512=ORIENTED_EDGE('',*,*,#4695,.T.);
#6513=ORIENTED_EDGE('',*,*,#4696,.F.);
#6514=ORIENTED_EDGE('',*,*,#4697,.T.);
#6515=ORIENTED_EDGE('',*,*,#4698,.F.);
#6516=ORIENTED_EDGE('',*,*,#4699,.T.);
#6517=ORIENTED_EDGE('',*,*,#4700,.T.);
#6518=ORIENTED_EDGE('',*,*,#4701,.T.);
#6519=ORIENTED_EDGE('',*,*,#4702,.F.);
#6520=ORIENTED_EDGE('',*,*,#4703,.F.);
#6521=ORIENTED_EDGE('',*,*,#4704,.T.);
#6522=ORIENTED_EDGE('',*,*,#4705,.T.);
#6523=ORIENTED_EDGE('',*,*,#4700,.F.);
#6524=ORIENTED_EDGE('',*,*,#4706,.F.);
#6525=ORIENTED_EDGE('',*,*,#4707,.T.);
#6526=ORIENTED_EDGE('',*,*,#4708,.T.);
#6527=ORIENTED_EDGE('',*,*,#4704,.F.);
#6528=ORIENTED_EDGE('',*,*,#4709,.F.);
#6529=ORIENTED_EDGE('',*,*,#4710,.T.);
#6530=ORIENTED_EDGE('',*,*,#4711,.T.);
#6531=ORIENTED_EDGE('',*,*,#4707,.F.);
#6532=ORIENTED_EDGE('',*,*,#4712,.F.);
#6533=ORIENTED_EDGE('',*,*,#4713,.T.);
#6534=ORIENTED_EDGE('',*,*,#4714,.T.);
#6535=ORIENTED_EDGE('',*,*,#4710,.F.);
#6536=ORIENTED_EDGE('',*,*,#4715,.F.);
#6537=ORIENTED_EDGE('',*,*,#4716,.T.);
#6538=ORIENTED_EDGE('',*,*,#4717,.T.);
#6539=ORIENTED_EDGE('',*,*,#4713,.F.);
#6540=ORIENTED_EDGE('',*,*,#4718,.F.);
#6541=ORIENTED_EDGE('',*,*,#4719,.T.);
#6542=ORIENTED_EDGE('',*,*,#4720,.T.);
#6543=ORIENTED_EDGE('',*,*,#4716,.F.);
#6544=ORIENTED_EDGE('',*,*,#4721,.F.);
#6545=ORIENTED_EDGE('',*,*,#4722,.T.);
#6546=ORIENTED_EDGE('',*,*,#4723,.T.);
#6547=ORIENTED_EDGE('',*,*,#4719,.F.);
#6548=ORIENTED_EDGE('',*,*,#4724,.F.);
#6549=ORIENTED_EDGE('',*,*,#4725,.T.);
#6550=ORIENTED_EDGE('',*,*,#4726,.T.);
#6551=ORIENTED_EDGE('',*,*,#4722,.F.);
#6552=ORIENTED_EDGE('',*,*,#4727,.F.);
#6553=ORIENTED_EDGE('',*,*,#4728,.T.);
#6554=ORIENTED_EDGE('',*,*,#4729,.T.);
#6555=ORIENTED_EDGE('',*,*,#4725,.F.);
#6556=ORIENTED_EDGE('',*,*,#4730,.F.);
#6557=ORIENTED_EDGE('',*,*,#4731,.T.);
#6558=ORIENTED_EDGE('',*,*,#4732,.T.);
#6559=ORIENTED_EDGE('',*,*,#4728,.F.);
#6560=ORIENTED_EDGE('',*,*,#4733,.F.);
#6561=ORIENTED_EDGE('',*,*,#4734,.T.);
#6562=ORIENTED_EDGE('',*,*,#4735,.T.);
#6563=ORIENTED_EDGE('',*,*,#4731,.F.);
#6564=ORIENTED_EDGE('',*,*,#4736,.F.);
#6565=ORIENTED_EDGE('',*,*,#4737,.T.);
#6566=ORIENTED_EDGE('',*,*,#4738,.T.);
#6567=ORIENTED_EDGE('',*,*,#4734,.F.);
#6568=ORIENTED_EDGE('',*,*,#4739,.F.);
#6569=ORIENTED_EDGE('',*,*,#4740,.T.);
#6570=ORIENTED_EDGE('',*,*,#4741,.T.);
#6571=ORIENTED_EDGE('',*,*,#4737,.F.);
#6572=ORIENTED_EDGE('',*,*,#4742,.F.);
#6573=ORIENTED_EDGE('',*,*,#4743,.T.);
#6574=ORIENTED_EDGE('',*,*,#4744,.T.);
#6575=ORIENTED_EDGE('',*,*,#4740,.F.);
#6576=ORIENTED_EDGE('',*,*,#4745,.F.);
#6577=ORIENTED_EDGE('',*,*,#4746,.F.);
#6578=ORIENTED_EDGE('',*,*,#4747,.F.);
#6579=ORIENTED_EDGE('',*,*,#4748,.F.);
#6580=ORIENTED_EDGE('',*,*,#4749,.T.);
#6581=ORIENTED_EDGE('',*,*,#4652,.F.);
#6582=ORIENTED_EDGE('',*,*,#4750,.T.);
#6583=ORIENTED_EDGE('',*,*,#4702,.T.);
#6584=ORIENTED_EDGE('',*,*,#4751,.T.);
#6585=ORIENTED_EDGE('',*,*,#4746,.T.);
#6586=ORIENTED_EDGE('',*,*,#4752,.T.);
#6587=ORIENTED_EDGE('',*,*,#4743,.F.);
#6588=ORIENTED_EDGE('',*,*,#4753,.F.);
#6589=ORIENTED_EDGE('',*,*,#4751,.F.);
#6590=ORIENTED_EDGE('',*,*,#4701,.F.);
#6591=ORIENTED_EDGE('',*,*,#4705,.F.);
#6592=ORIENTED_EDGE('',*,*,#4708,.F.);
#6593=ORIENTED_EDGE('',*,*,#4711,.F.);
#6594=ORIENTED_EDGE('',*,*,#4714,.F.);
#6595=ORIENTED_EDGE('',*,*,#4717,.F.);
#6596=ORIENTED_EDGE('',*,*,#4720,.F.);
#6597=ORIENTED_EDGE('',*,*,#4723,.F.);
#6598=ORIENTED_EDGE('',*,*,#4726,.F.);
#6599=ORIENTED_EDGE('',*,*,#4729,.F.);
#6600=ORIENTED_EDGE('',*,*,#4732,.F.);
#6601=ORIENTED_EDGE('',*,*,#4735,.F.);
#6602=ORIENTED_EDGE('',*,*,#4738,.F.);
#6603=ORIENTED_EDGE('',*,*,#4741,.F.);
#6604=ORIENTED_EDGE('',*,*,#4744,.F.);
#6605=ORIENTED_EDGE('',*,*,#4752,.F.);
#6606=ORIENTED_EDGE('',*,*,#4749,.F.);
#6607=ORIENTED_EDGE('',*,*,#4754,.F.);
#6608=ORIENTED_EDGE('',*,*,#4697,.F.);
#6609=ORIENTED_EDGE('',*,*,#4755,.F.);
#6610=ORIENTED_EDGE('',*,*,#4695,.F.);
#6611=ORIENTED_EDGE('',*,*,#4692,.F.);
#6612=ORIENTED_EDGE('',*,*,#4689,.F.);
#6613=ORIENTED_EDGE('',*,*,#4686,.F.);
#6614=ORIENTED_EDGE('',*,*,#4683,.F.);
#6615=ORIENTED_EDGE('',*,*,#4680,.F.);
#6616=ORIENTED_EDGE('',*,*,#4677,.F.);
#6617=ORIENTED_EDGE('',*,*,#4674,.F.);
#6618=ORIENTED_EDGE('',*,*,#4671,.F.);
#6619=ORIENTED_EDGE('',*,*,#4668,.F.);
#6620=ORIENTED_EDGE('',*,*,#4665,.F.);
#6621=ORIENTED_EDGE('',*,*,#4662,.F.);
#6622=ORIENTED_EDGE('',*,*,#4659,.F.);
#6623=ORIENTED_EDGE('',*,*,#4656,.F.);
#6624=ORIENTED_EDGE('',*,*,#4653,.F.);
#6625=ORIENTED_EDGE('',*,*,#4750,.F.);
#6626=ORIENTED_EDGE('',*,*,#4651,.F.);
#6627=ORIENTED_EDGE('',*,*,#4658,.F.);
#6628=ORIENTED_EDGE('',*,*,#4661,.F.);
#6629=ORIENTED_EDGE('',*,*,#4664,.F.);
#6630=ORIENTED_EDGE('',*,*,#4667,.F.);
#6631=ORIENTED_EDGE('',*,*,#4670,.F.);
#6632=ORIENTED_EDGE('',*,*,#4673,.F.);
#6633=ORIENTED_EDGE('',*,*,#4676,.F.);
#6634=ORIENTED_EDGE('',*,*,#4679,.F.);
#6635=ORIENTED_EDGE('',*,*,#4682,.F.);
#6636=ORIENTED_EDGE('',*,*,#4685,.F.);
#6637=ORIENTED_EDGE('',*,*,#4688,.F.);
#6638=ORIENTED_EDGE('',*,*,#4691,.F.);
#6639=ORIENTED_EDGE('',*,*,#4694,.F.);
#6640=ORIENTED_EDGE('',*,*,#4756,.F.);
#6641=ORIENTED_EDGE('',*,*,#4699,.F.);
#6642=ORIENTED_EDGE('',*,*,#4757,.F.);
#6643=ORIENTED_EDGE('',*,*,#4747,.T.);
#6644=ORIENTED_EDGE('',*,*,#4753,.T.);
#6645=ORIENTED_EDGE('',*,*,#4745,.T.);
#6646=ORIENTED_EDGE('',*,*,#4742,.T.);
#6647=ORIENTED_EDGE('',*,*,#4739,.T.);
#6648=ORIENTED_EDGE('',*,*,#4736,.T.);
#6649=ORIENTED_EDGE('',*,*,#4733,.T.);
#6650=ORIENTED_EDGE('',*,*,#4730,.T.);
#6651=ORIENTED_EDGE('',*,*,#4727,.T.);
#6652=ORIENTED_EDGE('',*,*,#4724,.T.);
#6653=ORIENTED_EDGE('',*,*,#4721,.T.);
#6654=ORIENTED_EDGE('',*,*,#4718,.T.);
#6655=ORIENTED_EDGE('',*,*,#4715,.T.);
#6656=ORIENTED_EDGE('',*,*,#4712,.T.);
#6657=ORIENTED_EDGE('',*,*,#4709,.T.);
#6658=ORIENTED_EDGE('',*,*,#4706,.T.);
#6659=ORIENTED_EDGE('',*,*,#4703,.T.);
#6660=ORIENTED_EDGE('',*,*,#4696,.T.);
#6661=ORIENTED_EDGE('',*,*,#4756,.T.);
#6662=ORIENTED_EDGE('',*,*,#4693,.F.);
#6663=ORIENTED_EDGE('',*,*,#4755,.T.);
#6664=ORIENTED_EDGE('',*,*,#4655,.F.);
#6665=ORIENTED_EDGE('',*,*,#4758,.T.);
#6666=ORIENTED_EDGE('',*,*,#4759,.T.);
#6667=ORIENTED_EDGE('',*,*,#4760,.F.);
#6668=ORIENTED_EDGE('',*,*,#4761,.F.);
#6669=ORIENTED_EDGE('',*,*,#4762,.T.);
#6670=ORIENTED_EDGE('',*,*,#4763,.T.);
#6671=ORIENTED_EDGE('',*,*,#4764,.F.);
#6672=ORIENTED_EDGE('',*,*,#4759,.F.);
#6673=ORIENTED_EDGE('',*,*,#4765,.T.);
#6674=ORIENTED_EDGE('',*,*,#4766,.T.);
#6675=ORIENTED_EDGE('',*,*,#4767,.F.);
#6676=ORIENTED_EDGE('',*,*,#4763,.F.);
#6677=ORIENTED_EDGE('',*,*,#4768,.T.);
#6678=ORIENTED_EDGE('',*,*,#4761,.T.);
#6679=ORIENTED_EDGE('',*,*,#4769,.F.);
#6680=ORIENTED_EDGE('',*,*,#4766,.F.);
#6681=ORIENTED_EDGE('',*,*,#4768,.F.);
#6682=ORIENTED_EDGE('',*,*,#4765,.F.);
#6683=ORIENTED_EDGE('',*,*,#4762,.F.);
#6684=ORIENTED_EDGE('',*,*,#4758,.F.);
#6685=ORIENTED_EDGE('',*,*,#4770,.T.);
#6686=ORIENTED_EDGE('',*,*,#4771,.T.);
#6687=ORIENTED_EDGE('',*,*,#4772,.F.);
#6688=ORIENTED_EDGE('',*,*,#4771,.F.);
#6689=ORIENTED_EDGE('',*,*,#4773,.F.);
#6690=ORIENTED_EDGE('',*,*,#4770,.F.);
#6691=ORIENTED_EDGE('',*,*,#4774,.F.);
#6692=ORIENTED_EDGE('',*,*,#4772,.T.);
#6693=ORIENTED_EDGE('',*,*,#4775,.F.);
#6694=ORIENTED_EDGE('',*,*,#4776,.T.);
#6695=ORIENTED_EDGE('',*,*,#4774,.T.);
#6696=ORIENTED_EDGE('',*,*,#4776,.F.);
#6697=ORIENTED_EDGE('',*,*,#4777,.F.);
#6698=ORIENTED_EDGE('',*,*,#4778,.T.);
#6699=ORIENTED_EDGE('',*,*,#4779,.F.);
#6700=ORIENTED_EDGE('',*,*,#4780,.F.);
#6701=ORIENTED_EDGE('',*,*,#4781,.F.);
#6702=ORIENTED_EDGE('',*,*,#4780,.T.);
#6703=ORIENTED_EDGE('',*,*,#4782,.F.);
#6704=ORIENTED_EDGE('',*,*,#4783,.F.);
#6705=ORIENTED_EDGE('',*,*,#4784,.F.);
#6706=ORIENTED_EDGE('',*,*,#4783,.T.);
#6707=ORIENTED_EDGE('',*,*,#4785,.F.);
#6708=ORIENTED_EDGE('',*,*,#4786,.F.);
#6709=ORIENTED_EDGE('',*,*,#4787,.F.);
#6710=ORIENTED_EDGE('',*,*,#4786,.T.);
#6711=ORIENTED_EDGE('',*,*,#4788,.F.);
#6712=ORIENTED_EDGE('',*,*,#4789,.F.);
#6713=ORIENTED_EDGE('',*,*,#4790,.F.);
#6714=ORIENTED_EDGE('',*,*,#4789,.T.);
#6715=ORIENTED_EDGE('',*,*,#4791,.F.);
#6716=ORIENTED_EDGE('',*,*,#4792,.F.);
#6717=ORIENTED_EDGE('',*,*,#4793,.F.);
#6718=ORIENTED_EDGE('',*,*,#4792,.T.);
#6719=ORIENTED_EDGE('',*,*,#4794,.F.);
#6720=ORIENTED_EDGE('',*,*,#4778,.F.);
#6721=ORIENTED_EDGE('',*,*,#4794,.T.);
#6722=ORIENTED_EDGE('',*,*,#4791,.T.);
#6723=ORIENTED_EDGE('',*,*,#4788,.T.);
#6724=ORIENTED_EDGE('',*,*,#4785,.T.);
#6725=ORIENTED_EDGE('',*,*,#4782,.T.);
#6726=ORIENTED_EDGE('',*,*,#4779,.T.);
#6727=ORIENTED_EDGE('',*,*,#4757,.T.);
#6728=ORIENTED_EDGE('',*,*,#4698,.T.);
#6729=ORIENTED_EDGE('',*,*,#4754,.T.);
#6730=ORIENTED_EDGE('',*,*,#4748,.T.);
#6731=ORIENTED_EDGE('',*,*,#4795,.T.);
#6732=ORIENTED_EDGE('',*,*,#4796,.F.);
#6733=ORIENTED_EDGE('',*,*,#4795,.F.);
#6734=ORIENTED_EDGE('',*,*,#4797,.T.);
#6735=ORIENTED_EDGE('',*,*,#4798,.T.);
#6736=ORIENTED_EDGE('',*,*,#4797,.F.);
#6737=ORIENTED_EDGE('',*,*,#4798,.F.);
#6738=ORIENTED_EDGE('',*,*,#4760,.T.);
#6739=ORIENTED_EDGE('',*,*,#4764,.T.);
#6740=ORIENTED_EDGE('',*,*,#4767,.T.);
#6741=ORIENTED_EDGE('',*,*,#4769,.T.);
#6742=ORIENTED_EDGE('',*,*,#4773,.T.);
#6743=ORIENTED_EDGE('',*,*,#4799,.T.);
#6744=ORIENTED_EDGE('',*,*,#4796,.T.);
#6745=ORIENTED_EDGE('',*,*,#4799,.F.);
#6746=ORIENTED_EDGE('',*,*,#4775,.T.);
#6747=ORIENTED_EDGE('',*,*,#4777,.T.);
#6748=ORIENTED_EDGE('',*,*,#4781,.T.);
#6749=ORIENTED_EDGE('',*,*,#4784,.T.);
#6750=ORIENTED_EDGE('',*,*,#4787,.T.);
#6751=ORIENTED_EDGE('',*,*,#4790,.T.);
#6752=ORIENTED_EDGE('',*,*,#4793,.T.);
#6753=ORIENTED_EDGE('',*,*,#4800,.F.);
#6754=ORIENTED_EDGE('',*,*,#4801,.T.);
#6755=ORIENTED_EDGE('',*,*,#4802,.F.);
#6756=ORIENTED_EDGE('',*,*,#4803,.F.);
#6757=ORIENTED_EDGE('',*,*,#4804,.F.);
#6758=ORIENTED_EDGE('',*,*,#4805,.T.);
#6759=ORIENTED_EDGE('',*,*,#4806,.F.);
#6760=ORIENTED_EDGE('',*,*,#4801,.F.);
#6761=ORIENTED_EDGE('',*,*,#4807,.F.);
#6762=ORIENTED_EDGE('',*,*,#4808,.T.);
#6763=ORIENTED_EDGE('',*,*,#4809,.F.);
#6764=ORIENTED_EDGE('',*,*,#4805,.F.);
#6765=ORIENTED_EDGE('',*,*,#4810,.F.);
#6766=ORIENTED_EDGE('',*,*,#4811,.T.);
#6767=ORIENTED_EDGE('',*,*,#4812,.F.);
#6768=ORIENTED_EDGE('',*,*,#4808,.F.);
#6769=ORIENTED_EDGE('',*,*,#4813,.F.);
#6770=ORIENTED_EDGE('',*,*,#4814,.T.);
#6771=ORIENTED_EDGE('',*,*,#4815,.F.);
#6772=ORIENTED_EDGE('',*,*,#4811,.F.);
#6773=ORIENTED_EDGE('',*,*,#4816,.F.);
#6774=ORIENTED_EDGE('',*,*,#4803,.T.);
#6775=ORIENTED_EDGE('',*,*,#4817,.F.);
#6776=ORIENTED_EDGE('',*,*,#4814,.F.);
#6777=ORIENTED_EDGE('',*,*,#4818,.T.);
#6778=ORIENTED_EDGE('',*,*,#4819,.T.);
#6779=ORIENTED_EDGE('',*,*,#4820,.F.);
#6780=ORIENTED_EDGE('',*,*,#4821,.F.);
#6781=ORIENTED_EDGE('',*,*,#4822,.T.);
#6782=ORIENTED_EDGE('',*,*,#4821,.T.);
#6783=ORIENTED_EDGE('',*,*,#4823,.F.);
#6784=ORIENTED_EDGE('',*,*,#4824,.F.);
#6785=ORIENTED_EDGE('',*,*,#4825,.T.);
#6786=ORIENTED_EDGE('',*,*,#4824,.T.);
#6787=ORIENTED_EDGE('',*,*,#4826,.F.);
#6788=ORIENTED_EDGE('',*,*,#4827,.F.);
#6789=ORIENTED_EDGE('',*,*,#4828,.T.);
#6790=ORIENTED_EDGE('',*,*,#4827,.T.);
#6791=ORIENTED_EDGE('',*,*,#4829,.F.);
#6792=ORIENTED_EDGE('',*,*,#4819,.F.);
#6793=ORIENTED_EDGE('',*,*,#4829,.T.);
#6794=ORIENTED_EDGE('',*,*,#4826,.T.);
#6795=ORIENTED_EDGE('',*,*,#4823,.T.);
#6796=ORIENTED_EDGE('',*,*,#4820,.T.);
#6797=ORIENTED_EDGE('',*,*,#4800,.T.);
#6798=ORIENTED_EDGE('',*,*,#4816,.T.);
#6799=ORIENTED_EDGE('',*,*,#4813,.T.);
#6800=ORIENTED_EDGE('',*,*,#4810,.T.);
#6801=ORIENTED_EDGE('',*,*,#4807,.T.);
#6802=ORIENTED_EDGE('',*,*,#4804,.T.);
#6803=ORIENTED_EDGE('',*,*,#4828,.F.);
#6804=ORIENTED_EDGE('',*,*,#4818,.F.);
#6805=ORIENTED_EDGE('',*,*,#4822,.F.);
#6806=ORIENTED_EDGE('',*,*,#4825,.F.);
#6807=ORIENTED_EDGE('',*,*,#4802,.T.);
#6808=ORIENTED_EDGE('',*,*,#4806,.T.);
#6809=ORIENTED_EDGE('',*,*,#4809,.T.);
#6810=ORIENTED_EDGE('',*,*,#4812,.T.);
#6811=ORIENTED_EDGE('',*,*,#4815,.T.);
#6812=ORIENTED_EDGE('',*,*,#4817,.T.);
#6813=ORIENTED_EDGE('',*,*,#4830,.F.);
#6814=ORIENTED_EDGE('',*,*,#4831,.T.);
#6815=ORIENTED_EDGE('',*,*,#4832,.T.);
#6816=ORIENTED_EDGE('',*,*,#4831,.F.);
#6817=ORIENTED_EDGE('',*,*,#4833,.F.);
#6818=ORIENTED_EDGE('',*,*,#4834,.T.);
#6819=ORIENTED_EDGE('',*,*,#4835,.T.);
#6820=ORIENTED_EDGE('',*,*,#4834,.F.);
#6821=ORIENTED_EDGE('',*,*,#4833,.T.);
#6822=ORIENTED_EDGE('',*,*,#4830,.T.);
#6823=ORIENTED_EDGE('',*,*,#4835,.F.);
#6824=ORIENTED_EDGE('',*,*,#4832,.F.);
#6825=ORIENTED_EDGE('',*,*,#4836,.F.);
#6826=ORIENTED_EDGE('',*,*,#4837,.F.);
#6827=ORIENTED_EDGE('',*,*,#4838,.F.);
#6828=ORIENTED_EDGE('',*,*,#4839,.F.);
#6829=ORIENTED_EDGE('',*,*,#4840,.F.);
#6830=ORIENTED_EDGE('',*,*,#4841,.F.);
#6831=ORIENTED_EDGE('',*,*,#4842,.F.);
#6832=ORIENTED_EDGE('',*,*,#4843,.F.);
#6833=ORIENTED_EDGE('',*,*,#4843,.T.);
#6834=ORIENTED_EDGE('',*,*,#4844,.F.);
#6835=ORIENTED_EDGE('',*,*,#4837,.T.);
#6836=ORIENTED_EDGE('',*,*,#4845,.F.);
#6837=ORIENTED_EDGE('',*,*,#4840,.T.);
#6838=ORIENTED_EDGE('',*,*,#4845,.T.);
#6839=ORIENTED_EDGE('',*,*,#4836,.T.);
#6840=ORIENTED_EDGE('',*,*,#4846,.F.);
#6841=ORIENTED_EDGE('',*,*,#4842,.T.);
#6842=ORIENTED_EDGE('',*,*,#4847,.F.);
#6843=ORIENTED_EDGE('',*,*,#4838,.T.);
#6844=ORIENTED_EDGE('',*,*,#4844,.T.);
#6845=ORIENTED_EDGE('',*,*,#4841,.T.);
#6846=ORIENTED_EDGE('',*,*,#4846,.T.);
#6847=ORIENTED_EDGE('',*,*,#4839,.T.);
#6848=ORIENTED_EDGE('',*,*,#4847,.T.);
#6849=ORIENTED_EDGE('',*,*,#4848,.F.);
#6850=ORIENTED_EDGE('',*,*,#4849,.T.);
#6851=ORIENTED_EDGE('',*,*,#4850,.T.);
#6852=ORIENTED_EDGE('',*,*,#4849,.F.);
#6853=ORIENTED_EDGE('',*,*,#4851,.F.);
#6854=ORIENTED_EDGE('',*,*,#4852,.T.);
#6855=ORIENTED_EDGE('',*,*,#4853,.T.);
#6856=ORIENTED_EDGE('',*,*,#4852,.F.);
#6857=ORIENTED_EDGE('',*,*,#4851,.T.);
#6858=ORIENTED_EDGE('',*,*,#4848,.T.);
#6859=ORIENTED_EDGE('',*,*,#4853,.F.);
#6860=ORIENTED_EDGE('',*,*,#4850,.F.);
#6861=ORIENTED_EDGE('',*,*,#4854,.F.);
#6862=ORIENTED_EDGE('',*,*,#4855,.T.);
#6863=ORIENTED_EDGE('',*,*,#4856,.T.);
#6864=ORIENTED_EDGE('',*,*,#4857,.T.);
#6865=ORIENTED_EDGE('',*,*,#4858,.F.);
#6866=ORIENTED_EDGE('',*,*,#4859,.T.);
#6867=ORIENTED_EDGE('',*,*,#4854,.T.);
#6868=ORIENTED_EDGE('',*,*,#4860,.T.);
#6869=ORIENTED_EDGE('',*,*,#4861,.F.);
#6870=ORIENTED_EDGE('',*,*,#4862,.T.);
#6871=ORIENTED_EDGE('',*,*,#4858,.T.);
#6872=ORIENTED_EDGE('',*,*,#4863,.T.);
#6873=ORIENTED_EDGE('',*,*,#4864,.F.);
#6874=ORIENTED_EDGE('',*,*,#4865,.T.);
#6875=ORIENTED_EDGE('',*,*,#4861,.T.);
#6876=ORIENTED_EDGE('',*,*,#4866,.T.);
#6877=ORIENTED_EDGE('',*,*,#4867,.F.);
#6878=ORIENTED_EDGE('',*,*,#4868,.T.);
#6879=ORIENTED_EDGE('',*,*,#4864,.T.);
#6880=ORIENTED_EDGE('',*,*,#4869,.T.);
#6881=ORIENTED_EDGE('',*,*,#4870,.F.);
#6882=ORIENTED_EDGE('',*,*,#4871,.T.);
#6883=ORIENTED_EDGE('',*,*,#4867,.T.);
#6884=ORIENTED_EDGE('',*,*,#4872,.T.);
#6885=ORIENTED_EDGE('',*,*,#4873,.F.);
#6886=ORIENTED_EDGE('',*,*,#4874,.T.);
#6887=ORIENTED_EDGE('',*,*,#4870,.T.);
#6888=ORIENTED_EDGE('',*,*,#4875,.T.);
#6889=ORIENTED_EDGE('',*,*,#4876,.F.);
#6890=ORIENTED_EDGE('',*,*,#4877,.T.);
#6891=ORIENTED_EDGE('',*,*,#4873,.T.);
#6892=ORIENTED_EDGE('',*,*,#4878,.T.);
#6893=ORIENTED_EDGE('',*,*,#4879,.F.);
#6894=ORIENTED_EDGE('',*,*,#4880,.T.);
#6895=ORIENTED_EDGE('',*,*,#4876,.T.);
#6896=ORIENTED_EDGE('',*,*,#4881,.T.);
#6897=ORIENTED_EDGE('',*,*,#4882,.F.);
#6898=ORIENTED_EDGE('',*,*,#4883,.T.);
#6899=ORIENTED_EDGE('',*,*,#4879,.T.);
#6900=ORIENTED_EDGE('',*,*,#4884,.T.);
#6901=ORIENTED_EDGE('',*,*,#4885,.F.);
#6902=ORIENTED_EDGE('',*,*,#4886,.T.);
#6903=ORIENTED_EDGE('',*,*,#4887,.T.);
#6904=ORIENTED_EDGE('',*,*,#4888,.F.);
#6905=ORIENTED_EDGE('',*,*,#4889,.F.);
#6906=ORIENTED_EDGE('',*,*,#4890,.T.);
#6907=ORIENTED_EDGE('',*,*,#4885,.T.);
#6908=ORIENTED_EDGE('',*,*,#4891,.F.);
#6909=ORIENTED_EDGE('',*,*,#4892,.F.);
#6910=ORIENTED_EDGE('',*,*,#4893,.T.);
#6911=ORIENTED_EDGE('',*,*,#4889,.T.);
#6912=ORIENTED_EDGE('',*,*,#4894,.F.);
#6913=ORIENTED_EDGE('',*,*,#4895,.F.);
#6914=ORIENTED_EDGE('',*,*,#4896,.T.);
#6915=ORIENTED_EDGE('',*,*,#4892,.T.);
#6916=ORIENTED_EDGE('',*,*,#4897,.F.);
#6917=ORIENTED_EDGE('',*,*,#4898,.F.);
#6918=ORIENTED_EDGE('',*,*,#4899,.T.);
#6919=ORIENTED_EDGE('',*,*,#4895,.T.);
#6920=ORIENTED_EDGE('',*,*,#4900,.F.);
#6921=ORIENTED_EDGE('',*,*,#4901,.F.);
#6922=ORIENTED_EDGE('',*,*,#4902,.T.);
#6923=ORIENTED_EDGE('',*,*,#4898,.T.);
#6924=ORIENTED_EDGE('',*,*,#4903,.F.);
#6925=ORIENTED_EDGE('',*,*,#4904,.F.);
#6926=ORIENTED_EDGE('',*,*,#4905,.T.);
#6927=ORIENTED_EDGE('',*,*,#4901,.T.);
#6928=ORIENTED_EDGE('',*,*,#4906,.F.);
#6929=ORIENTED_EDGE('',*,*,#4907,.F.);
#6930=ORIENTED_EDGE('',*,*,#4908,.T.);
#6931=ORIENTED_EDGE('',*,*,#4904,.T.);
#6932=ORIENTED_EDGE('',*,*,#4909,.F.);
#6933=ORIENTED_EDGE('',*,*,#4910,.F.);
#6934=ORIENTED_EDGE('',*,*,#4911,.T.);
#6935=ORIENTED_EDGE('',*,*,#4907,.T.);
#6936=ORIENTED_EDGE('',*,*,#4912,.F.);
#6937=ORIENTED_EDGE('',*,*,#4913,.F.);
#6938=ORIENTED_EDGE('',*,*,#4914,.T.);
#6939=ORIENTED_EDGE('',*,*,#4910,.T.);
#6940=ORIENTED_EDGE('',*,*,#4915,.F.);
#6941=ORIENTED_EDGE('',*,*,#4916,.F.);
#6942=ORIENTED_EDGE('',*,*,#4887,.F.);
#6943=ORIENTED_EDGE('',*,*,#4917,.F.);
#6944=ORIENTED_EDGE('',*,*,#4918,.F.);
#6945=ORIENTED_EDGE('',*,*,#4919,.F.);
#6946=ORIENTED_EDGE('',*,*,#4920,.T.);
#6947=ORIENTED_EDGE('',*,*,#4921,.F.);
#6948=ORIENTED_EDGE('',*,*,#4920,.F.);
#6949=ORIENTED_EDGE('',*,*,#4917,.T.);
#6950=ORIENTED_EDGE('',*,*,#4886,.F.);
#6951=ORIENTED_EDGE('',*,*,#4890,.F.);
#6952=ORIENTED_EDGE('',*,*,#4893,.F.);
#6953=ORIENTED_EDGE('',*,*,#4896,.F.);
#6954=ORIENTED_EDGE('',*,*,#4899,.F.);
#6955=ORIENTED_EDGE('',*,*,#4902,.F.);
#6956=ORIENTED_EDGE('',*,*,#4905,.F.);
#6957=ORIENTED_EDGE('',*,*,#4908,.F.);
#6958=ORIENTED_EDGE('',*,*,#4911,.F.);
#6959=ORIENTED_EDGE('',*,*,#4914,.F.);
#6960=ORIENTED_EDGE('',*,*,#4922,.F.);
#6961=ORIENTED_EDGE('',*,*,#4923,.F.);
#6962=ORIENTED_EDGE('',*,*,#4855,.F.);
#6963=ORIENTED_EDGE('',*,*,#4859,.F.);
#6964=ORIENTED_EDGE('',*,*,#4862,.F.);
#6965=ORIENTED_EDGE('',*,*,#4865,.F.);
#6966=ORIENTED_EDGE('',*,*,#4868,.F.);
#6967=ORIENTED_EDGE('',*,*,#4871,.F.);
#6968=ORIENTED_EDGE('',*,*,#4874,.F.);
#6969=ORIENTED_EDGE('',*,*,#4877,.F.);
#6970=ORIENTED_EDGE('',*,*,#4880,.F.);
#6971=ORIENTED_EDGE('',*,*,#4883,.F.);
#6972=ORIENTED_EDGE('',*,*,#4924,.F.);
#6973=ORIENTED_EDGE('',*,*,#4913,.T.);
#6974=ORIENTED_EDGE('',*,*,#4925,.F.);
#6975=ORIENTED_EDGE('',*,*,#4926,.F.);
#6976=ORIENTED_EDGE('',*,*,#4922,.T.);
#6977=ORIENTED_EDGE('',*,*,#4916,.T.);
#6978=ORIENTED_EDGE('',*,*,#4919,.T.);
#6979=ORIENTED_EDGE('',*,*,#4927,.F.);
#6980=ORIENTED_EDGE('',*,*,#4884,.F.);
#6981=ORIENTED_EDGE('',*,*,#4881,.F.);
#6982=ORIENTED_EDGE('',*,*,#4878,.F.);
#6983=ORIENTED_EDGE('',*,*,#4875,.F.);
#6984=ORIENTED_EDGE('',*,*,#4872,.F.);
#6985=ORIENTED_EDGE('',*,*,#4869,.F.);
#6986=ORIENTED_EDGE('',*,*,#4866,.F.);
#6987=ORIENTED_EDGE('',*,*,#4863,.F.);
#6988=ORIENTED_EDGE('',*,*,#4860,.F.);
#6989=ORIENTED_EDGE('',*,*,#4857,.F.);
#6990=ORIENTED_EDGE('',*,*,#4928,.F.);
#6991=ORIENTED_EDGE('',*,*,#4925,.T.);
#6992=ORIENTED_EDGE('',*,*,#4915,.T.);
#6993=ORIENTED_EDGE('',*,*,#4912,.T.);
#6994=ORIENTED_EDGE('',*,*,#4909,.T.);
#6995=ORIENTED_EDGE('',*,*,#4906,.T.);
#6996=ORIENTED_EDGE('',*,*,#4903,.T.);
#6997=ORIENTED_EDGE('',*,*,#4900,.T.);
#6998=ORIENTED_EDGE('',*,*,#4897,.T.);
#6999=ORIENTED_EDGE('',*,*,#4894,.T.);
#7000=ORIENTED_EDGE('',*,*,#4891,.T.);
#7001=ORIENTED_EDGE('',*,*,#4888,.T.);
#7002=ORIENTED_EDGE('',*,*,#4882,.T.);
#7003=ORIENTED_EDGE('',*,*,#4927,.T.);
#7004=ORIENTED_EDGE('',*,*,#4918,.T.);
#7005=ORIENTED_EDGE('',*,*,#4924,.T.);
#7006=ORIENTED_EDGE('',*,*,#4929,.F.);
#7007=ORIENTED_EDGE('',*,*,#4930,.T.);
#7008=ORIENTED_EDGE('',*,*,#4931,.T.);
#7009=ORIENTED_EDGE('',*,*,#4932,.F.);
#7010=ORIENTED_EDGE('',*,*,#4933,.F.);
#7011=ORIENTED_EDGE('',*,*,#4934,.T.);
#7012=ORIENTED_EDGE('',*,*,#4935,.T.);
#7013=ORIENTED_EDGE('',*,*,#4930,.F.);
#7014=ORIENTED_EDGE('',*,*,#4936,.F.);
#7015=ORIENTED_EDGE('',*,*,#4937,.T.);
#7016=ORIENTED_EDGE('',*,*,#4938,.T.);
#7017=ORIENTED_EDGE('',*,*,#4934,.F.);
#7018=ORIENTED_EDGE('',*,*,#4939,.F.);
#7019=ORIENTED_EDGE('',*,*,#4940,.T.);
#7020=ORIENTED_EDGE('',*,*,#4941,.T.);
#7021=ORIENTED_EDGE('',*,*,#4937,.F.);
#7022=ORIENTED_EDGE('',*,*,#4942,.F.);
#7023=ORIENTED_EDGE('',*,*,#4943,.T.);
#7024=ORIENTED_EDGE('',*,*,#4944,.T.);
#7025=ORIENTED_EDGE('',*,*,#4940,.F.);
#7026=ORIENTED_EDGE('',*,*,#4945,.F.);
#7027=ORIENTED_EDGE('',*,*,#4932,.T.);
#7028=ORIENTED_EDGE('',*,*,#4946,.T.);
#7029=ORIENTED_EDGE('',*,*,#4943,.F.);
#7030=ORIENTED_EDGE('',*,*,#4946,.F.);
#7031=ORIENTED_EDGE('',*,*,#4931,.F.);
#7032=ORIENTED_EDGE('',*,*,#4935,.F.);
#7033=ORIENTED_EDGE('',*,*,#4938,.F.);
#7034=ORIENTED_EDGE('',*,*,#4941,.F.);
#7035=ORIENTED_EDGE('',*,*,#4944,.F.);
#7036=ORIENTED_EDGE('',*,*,#4947,.T.);
#7037=ORIENTED_EDGE('',*,*,#4923,.T.);
#7038=ORIENTED_EDGE('',*,*,#4926,.T.);
#7039=ORIENTED_EDGE('',*,*,#4928,.T.);
#7040=ORIENTED_EDGE('',*,*,#4856,.F.);
#7041=ORIENTED_EDGE('',*,*,#4947,.F.);
#7042=ORIENTED_EDGE('',*,*,#4948,.T.);
#7043=ORIENTED_EDGE('',*,*,#4949,.T.);
#7044=ORIENTED_EDGE('',*,*,#4948,.F.);
#7045=ORIENTED_EDGE('',*,*,#4949,.F.);
#7046=ORIENTED_EDGE('',*,*,#4929,.T.);
#7047=ORIENTED_EDGE('',*,*,#4945,.T.);
#7048=ORIENTED_EDGE('',*,*,#4942,.T.);
#7049=ORIENTED_EDGE('',*,*,#4939,.T.);
#7050=ORIENTED_EDGE('',*,*,#4936,.T.);
#7051=ORIENTED_EDGE('',*,*,#4933,.T.);
#7052=ORIENTED_EDGE('',*,*,#4921,.T.);
#7053=ORIENTED_EDGE('',*,*,#4950,.F.);
#7054=ORIENTED_EDGE('',*,*,#4951,.T.);
#7055=ORIENTED_EDGE('',*,*,#4952,.F.);
#7056=ORIENTED_EDGE('',*,*,#4953,.F.);
#7057=ORIENTED_EDGE('',*,*,#4954,.T.);
#7058=ORIENTED_EDGE('',*,*,#4950,.T.);
#7059=ORIENTED_EDGE('',*,*,#4955,.T.);
#7060=ORIENTED_EDGE('',*,*,#4956,.T.);
#7061=ORIENTED_EDGE('',*,*,#4957,.T.);
#7062=ORIENTED_EDGE('',*,*,#4958,.T.);
#7063=ORIENTED_EDGE('',*,*,#4959,.T.);
#7064=ORIENTED_EDGE('',*,*,#4960,.T.);
#7065=ORIENTED_EDGE('',*,*,#4961,.T.);
#7066=ORIENTED_EDGE('',*,*,#4962,.T.);
#7067=ORIENTED_EDGE('',*,*,#4962,.F.);
#7068=ORIENTED_EDGE('',*,*,#4963,.T.);
#7069=ORIENTED_EDGE('',*,*,#4964,.F.);
#7070=ORIENTED_EDGE('',*,*,#4963,.F.);
#7071=ORIENTED_EDGE('',*,*,#4961,.F.);
#7072=ORIENTED_EDGE('',*,*,#4965,.T.);
#7073=ORIENTED_EDGE('',*,*,#4966,.F.);
#7074=ORIENTED_EDGE('',*,*,#4965,.F.);
#7075=ORIENTED_EDGE('',*,*,#4967,.F.);
#7076=ORIENTED_EDGE('',*,*,#4968,.F.);
#7077=ORIENTED_EDGE('',*,*,#4956,.F.);
#7078=ORIENTED_EDGE('',*,*,#4969,.T.);
#7079=ORIENTED_EDGE('',*,*,#4970,.F.);
#7080=ORIENTED_EDGE('',*,*,#4971,.T.);
#7081=ORIENTED_EDGE('',*,*,#4972,.T.);
#7082=ORIENTED_EDGE('',*,*,#4971,.F.);
#7083=ORIENTED_EDGE('',*,*,#4969,.F.);
#7084=ORIENTED_EDGE('',*,*,#4955,.F.);
#7085=ORIENTED_EDGE('',*,*,#4953,.T.);
#7086=ORIENTED_EDGE('',*,*,#4973,.F.);
#7087=ORIENTED_EDGE('',*,*,#4972,.F.);
#7088=ORIENTED_EDGE('',*,*,#4974,.F.);
#7089=ORIENTED_EDGE('',*,*,#4951,.F.);
#7090=ORIENTED_EDGE('',*,*,#4954,.F.);
#7091=ORIENTED_EDGE('',*,*,#4975,.T.);
#7092=ORIENTED_EDGE('',*,*,#4976,.T.);
#7093=ORIENTED_EDGE('',*,*,#4976,.F.);
#7094=ORIENTED_EDGE('',*,*,#4977,.T.);
#7095=ORIENTED_EDGE('',*,*,#4978,.T.);
#7096=ORIENTED_EDGE('',*,*,#4977,.F.);
#7097=ORIENTED_EDGE('',*,*,#4979,.F.);
#7098=ORIENTED_EDGE('',*,*,#4975,.F.);
#7099=ORIENTED_EDGE('',*,*,#4960,.F.);
#7100=ORIENTED_EDGE('',*,*,#4980,.T.);
#7101=ORIENTED_EDGE('',*,*,#4980,.F.);
#7102=ORIENTED_EDGE('',*,*,#4959,.F.);
#7103=ORIENTED_EDGE('',*,*,#4981,.F.);
#7104=ORIENTED_EDGE('',*,*,#4982,.T.);
#7105=ORIENTED_EDGE('',*,*,#4978,.F.);
#7106=ORIENTED_EDGE('',*,*,#4983,.T.);
#7107=ORIENTED_EDGE('',*,*,#4984,.T.);
#7108=ORIENTED_EDGE('',*,*,#4957,.F.);
#7109=ORIENTED_EDGE('',*,*,#4968,.T.);
#7110=ORIENTED_EDGE('',*,*,#4970,.T.);
#7111=ORIENTED_EDGE('',*,*,#4985,.T.);
#7112=ORIENTED_EDGE('',*,*,#4981,.T.);
#7113=ORIENTED_EDGE('',*,*,#4958,.F.);
#7114=ORIENTED_EDGE('',*,*,#4984,.F.);
#7115=ORIENTED_EDGE('',*,*,#4974,.T.);
#7116=ORIENTED_EDGE('',*,*,#4979,.T.);
#7117=ORIENTED_EDGE('',*,*,#4982,.F.);
#7118=ORIENTED_EDGE('',*,*,#4985,.F.);
#7119=ORIENTED_EDGE('',*,*,#4983,.F.);
#7120=ORIENTED_EDGE('',*,*,#4967,.T.);
#7121=ORIENTED_EDGE('',*,*,#4973,.T.);
#7122=ORIENTED_EDGE('',*,*,#4952,.T.);
#7123=ORIENTED_EDGE('',*,*,#4964,.T.);
#7124=ORIENTED_EDGE('',*,*,#4966,.T.);
#7125=ORIENTED_EDGE('',*,*,#4986,.T.);
#7126=ORIENTED_EDGE('',*,*,#4987,.T.);
#7127=ORIENTED_EDGE('',*,*,#4988,.F.);
#7128=ORIENTED_EDGE('',*,*,#4987,.F.);
#7129=ORIENTED_EDGE('',*,*,#4989,.F.);
#7130=ORIENTED_EDGE('',*,*,#4986,.F.);
#7131=ORIENTED_EDGE('',*,*,#4990,.F.);
#7132=ORIENTED_EDGE('',*,*,#4988,.T.);
#7133=ORIENTED_EDGE('',*,*,#4991,.F.);
#7134=ORIENTED_EDGE('',*,*,#4992,.T.);
#7135=ORIENTED_EDGE('',*,*,#4990,.T.);
#7136=ORIENTED_EDGE('',*,*,#4992,.F.);
#7137=ORIENTED_EDGE('',*,*,#4993,.T.);
#7138=ORIENTED_EDGE('',*,*,#4994,.F.);
#7139=ORIENTED_EDGE('',*,*,#4993,.F.);
#7140=ORIENTED_EDGE('',*,*,#4995,.T.);
#7141=ORIENTED_EDGE('',*,*,#4996,.T.);
#7142=ORIENTED_EDGE('',*,*,#4995,.F.);
#7143=ORIENTED_EDGE('',*,*,#4996,.F.);
#7144=ORIENTED_EDGE('',*,*,#4989,.T.);
#7145=ORIENTED_EDGE('',*,*,#4997,.T.);
#7146=ORIENTED_EDGE('',*,*,#4994,.T.);
#7147=ORIENTED_EDGE('',*,*,#4997,.F.);
#7148=ORIENTED_EDGE('',*,*,#4991,.T.);
#7149=ORIENTED_EDGE('',*,*,#4998,.F.);
#7150=ORIENTED_EDGE('',*,*,#4999,.F.);
#7151=ORIENTED_EDGE('',*,*,#5000,.F.);
#7152=ORIENTED_EDGE('',*,*,#5001,.F.);
#7153=ORIENTED_EDGE('',*,*,#5002,.F.);
#7154=ORIENTED_EDGE('',*,*,#5003,.F.);
#7155=ORIENTED_EDGE('',*,*,#5004,.F.);
#7156=ORIENTED_EDGE('',*,*,#5005,.F.);
#7157=ORIENTED_EDGE('',*,*,#5005,.T.);
#7158=ORIENTED_EDGE('',*,*,#5006,.F.);
#7159=ORIENTED_EDGE('',*,*,#4999,.T.);
#7160=ORIENTED_EDGE('',*,*,#5007,.F.);
#7161=ORIENTED_EDGE('',*,*,#5002,.T.);
#7162=ORIENTED_EDGE('',*,*,#5007,.T.);
#7163=ORIENTED_EDGE('',*,*,#4998,.T.);
#7164=ORIENTED_EDGE('',*,*,#5008,.F.);
#7165=ORIENTED_EDGE('',*,*,#5004,.T.);
#7166=ORIENTED_EDGE('',*,*,#5009,.F.);
#7167=ORIENTED_EDGE('',*,*,#5000,.T.);
#7168=ORIENTED_EDGE('',*,*,#5006,.T.);
#7169=ORIENTED_EDGE('',*,*,#5003,.T.);
#7170=ORIENTED_EDGE('',*,*,#5008,.T.);
#7171=ORIENTED_EDGE('',*,*,#5001,.T.);
#7172=ORIENTED_EDGE('',*,*,#5009,.T.);
#7173=ORIENTED_EDGE('',*,*,#5010,.F.);
#7174=ORIENTED_EDGE('',*,*,#5011,.T.);
#7175=ORIENTED_EDGE('',*,*,#5012,.F.);
#7176=ORIENTED_EDGE('',*,*,#5013,.F.);
#7177=ORIENTED_EDGE('',*,*,#5014,.F.);
#7178=ORIENTED_EDGE('',*,*,#5015,.F.);
#7179=ORIENTED_EDGE('',*,*,#5016,.F.);
#7180=ORIENTED_EDGE('',*,*,#5017,.F.);
#7181=ORIENTED_EDGE('',*,*,#5012,.T.);
#7182=ORIENTED_EDGE('',*,*,#5018,.T.);
#7183=ORIENTED_EDGE('',*,*,#5019,.T.);
#7184=ORIENTED_EDGE('',*,*,#5020,.T.);
#7185=ORIENTED_EDGE('',*,*,#5016,.T.);
#7186=ORIENTED_EDGE('',*,*,#5021,.F.);
#7187=ORIENTED_EDGE('',*,*,#5022,.F.);
#7188=ORIENTED_EDGE('',*,*,#5023,.F.);
#7189=ORIENTED_EDGE('',*,*,#5024,.T.);
#7190=ORIENTED_EDGE('',*,*,#5025,.T.);
#7191=ORIENTED_EDGE('',*,*,#5015,.T.);
#7192=ORIENTED_EDGE('',*,*,#5026,.F.);
#7193=ORIENTED_EDGE('',*,*,#5027,.F.);
#7194=ORIENTED_EDGE('',*,*,#5021,.T.);
#7195=ORIENTED_EDGE('',*,*,#5028,.F.);
#7196=ORIENTED_EDGE('',*,*,#5029,.T.);
#7197=ORIENTED_EDGE('',*,*,#5025,.F.);
#7198=ORIENTED_EDGE('',*,*,#5029,.F.);
#7199=ORIENTED_EDGE('',*,*,#5030,.F.);
#7200=ORIENTED_EDGE('',*,*,#5031,.T.);
#7201=ORIENTED_EDGE('',*,*,#5024,.F.);
#7202=ORIENTED_EDGE('',*,*,#5031,.F.);
#7203=ORIENTED_EDGE('',*,*,#5032,.T.);
#7204=ORIENTED_EDGE('',*,*,#5033,.F.);
#7205=ORIENTED_EDGE('',*,*,#5017,.T.);
#7206=ORIENTED_EDGE('',*,*,#5020,.F.);
#7207=ORIENTED_EDGE('',*,*,#5034,.T.);
#7208=ORIENTED_EDGE('',*,*,#5034,.F.);
#7209=ORIENTED_EDGE('',*,*,#5035,.T.);
#7210=ORIENTED_EDGE('',*,*,#5036,.T.);
#7211=ORIENTED_EDGE('',*,*,#5035,.F.);
#7212=ORIENTED_EDGE('',*,*,#5037,.F.);
#7213=ORIENTED_EDGE('',*,*,#5032,.F.);
#7214=ORIENTED_EDGE('',*,*,#5019,.F.);
#7215=ORIENTED_EDGE('',*,*,#5038,.T.);
#7216=ORIENTED_EDGE('',*,*,#5018,.F.);
#7217=ORIENTED_EDGE('',*,*,#5011,.F.);
#7218=ORIENTED_EDGE('',*,*,#5039,.F.);
#7219=ORIENTED_EDGE('',*,*,#5038,.F.);
#7220=ORIENTED_EDGE('',*,*,#5036,.F.);
#7221=ORIENTED_EDGE('',*,*,#5022,.T.);
#7222=ORIENTED_EDGE('',*,*,#5027,.T.);
#7223=ORIENTED_EDGE('',*,*,#5040,.F.);
#7224=ORIENTED_EDGE('',*,*,#5041,.F.);
#7225=ORIENTED_EDGE('',*,*,#5013,.T.);
#7226=ORIENTED_EDGE('',*,*,#5023,.T.);
#7227=ORIENTED_EDGE('',*,*,#5041,.T.);
#7228=ORIENTED_EDGE('',*,*,#5042,.F.);
#7229=ORIENTED_EDGE('',*,*,#5010,.T.);
#7230=ORIENTED_EDGE('',*,*,#5042,.T.);
#7231=ORIENTED_EDGE('',*,*,#5040,.T.);
#7232=ORIENTED_EDGE('',*,*,#5026,.T.);
#7233=ORIENTED_EDGE('',*,*,#5014,.T.);
#7234=ORIENTED_EDGE('',*,*,#5033,.T.);
#7235=ORIENTED_EDGE('',*,*,#5037,.T.);
#7236=ORIENTED_EDGE('',*,*,#5039,.T.);
#7237=ORIENTED_EDGE('',*,*,#5028,.T.);
#7238=ORIENTED_EDGE('',*,*,#5030,.T.);
#7239=ORIENTED_EDGE('',*,*,#5043,.F.);
#7240=ORIENTED_EDGE('',*,*,#5044,.T.);
#7241=ORIENTED_EDGE('',*,*,#5045,.T.);
#7242=ORIENTED_EDGE('',*,*,#5044,.F.);
#7243=ORIENTED_EDGE('',*,*,#5046,.F.);
#7244=ORIENTED_EDGE('',*,*,#5047,.T.);
#7245=ORIENTED_EDGE('',*,*,#5048,.T.);
#7246=ORIENTED_EDGE('',*,*,#5047,.F.);
#7247=ORIENTED_EDGE('',*,*,#5046,.T.);
#7248=ORIENTED_EDGE('',*,*,#5043,.T.);
#7249=ORIENTED_EDGE('',*,*,#5048,.F.);
#7250=ORIENTED_EDGE('',*,*,#5045,.F.);
#7251=ORIENTED_EDGE('',*,*,#5049,.F.);
#7252=ORIENTED_EDGE('',*,*,#5050,.T.);
#7253=ORIENTED_EDGE('',*,*,#5051,.T.);
#7254=ORIENTED_EDGE('',*,*,#5052,.T.);
#7255=ORIENTED_EDGE('',*,*,#5053,.F.);
#7256=ORIENTED_EDGE('',*,*,#5054,.T.);
#7257=ORIENTED_EDGE('',*,*,#5049,.T.);
#7258=ORIENTED_EDGE('',*,*,#5055,.T.);
#7259=ORIENTED_EDGE('',*,*,#5056,.F.);
#7260=ORIENTED_EDGE('',*,*,#5057,.T.);
#7261=ORIENTED_EDGE('',*,*,#5053,.T.);
#7262=ORIENTED_EDGE('',*,*,#5058,.T.);
#7263=ORIENTED_EDGE('',*,*,#5059,.F.);
#7264=ORIENTED_EDGE('',*,*,#5060,.T.);
#7265=ORIENTED_EDGE('',*,*,#5056,.T.);
#7266=ORIENTED_EDGE('',*,*,#5061,.T.);
#7267=ORIENTED_EDGE('',*,*,#5062,.F.);
#7268=ORIENTED_EDGE('',*,*,#5063,.T.);
#7269=ORIENTED_EDGE('',*,*,#5059,.T.);
#7270=ORIENTED_EDGE('',*,*,#5064,.T.);
#7271=ORIENTED_EDGE('',*,*,#5065,.F.);
#7272=ORIENTED_EDGE('',*,*,#5066,.T.);
#7273=ORIENTED_EDGE('',*,*,#5062,.T.);
#7274=ORIENTED_EDGE('',*,*,#5067,.T.);
#7275=ORIENTED_EDGE('',*,*,#5068,.F.);
#7276=ORIENTED_EDGE('',*,*,#5069,.T.);
#7277=ORIENTED_EDGE('',*,*,#5065,.T.);
#7278=ORIENTED_EDGE('',*,*,#5070,.T.);
#7279=ORIENTED_EDGE('',*,*,#5071,.F.);
#7280=ORIENTED_EDGE('',*,*,#5072,.T.);
#7281=ORIENTED_EDGE('',*,*,#5068,.T.);
#7282=ORIENTED_EDGE('',*,*,#5073,.T.);
#7283=ORIENTED_EDGE('',*,*,#5074,.F.);
#7284=ORIENTED_EDGE('',*,*,#5075,.T.);
#7285=ORIENTED_EDGE('',*,*,#5071,.T.);
#7286=ORIENTED_EDGE('',*,*,#5076,.T.);
#7287=ORIENTED_EDGE('',*,*,#5077,.F.);
#7288=ORIENTED_EDGE('',*,*,#5078,.T.);
#7289=ORIENTED_EDGE('',*,*,#5074,.T.);
#7290=ORIENTED_EDGE('',*,*,#5079,.T.);
#7291=ORIENTED_EDGE('',*,*,#5080,.F.);
#7292=ORIENTED_EDGE('',*,*,#5081,.T.);
#7293=ORIENTED_EDGE('',*,*,#5077,.T.);
#7294=ORIENTED_EDGE('',*,*,#5082,.T.);
#7295=ORIENTED_EDGE('',*,*,#5083,.F.);
#7296=ORIENTED_EDGE('',*,*,#5084,.T.);
#7297=ORIENTED_EDGE('',*,*,#5080,.T.);
#7298=ORIENTED_EDGE('',*,*,#5085,.T.);
#7299=ORIENTED_EDGE('',*,*,#5086,.F.);
#7300=ORIENTED_EDGE('',*,*,#5087,.T.);
#7301=ORIENTED_EDGE('',*,*,#5083,.T.);
#7302=ORIENTED_EDGE('',*,*,#5088,.T.);
#7303=ORIENTED_EDGE('',*,*,#5089,.F.);
#7304=ORIENTED_EDGE('',*,*,#5090,.T.);
#7305=ORIENTED_EDGE('',*,*,#5086,.T.);
#7306=ORIENTED_EDGE('',*,*,#5091,.T.);
#7307=ORIENTED_EDGE('',*,*,#5092,.F.);
#7308=ORIENTED_EDGE('',*,*,#5093,.T.);
#7309=ORIENTED_EDGE('',*,*,#5089,.T.);
#7310=ORIENTED_EDGE('',*,*,#5094,.T.);
#7311=ORIENTED_EDGE('',*,*,#5095,.F.);
#7312=ORIENTED_EDGE('',*,*,#5096,.T.);
#7313=ORIENTED_EDGE('',*,*,#5092,.T.);
#7314=ORIENTED_EDGE('',*,*,#5097,.T.);
#7315=ORIENTED_EDGE('',*,*,#5098,.F.);
#7316=ORIENTED_EDGE('',*,*,#5099,.T.);
#7317=ORIENTED_EDGE('',*,*,#5095,.T.);
#7318=ORIENTED_EDGE('',*,*,#5100,.T.);
#7319=ORIENTED_EDGE('',*,*,#5101,.F.);
#7320=ORIENTED_EDGE('',*,*,#5102,.T.);
#7321=ORIENTED_EDGE('',*,*,#5098,.T.);
#7322=ORIENTED_EDGE('',*,*,#5103,.T.);
#7323=ORIENTED_EDGE('',*,*,#5104,.F.);
#7324=ORIENTED_EDGE('',*,*,#5105,.T.);
#7325=ORIENTED_EDGE('',*,*,#5101,.T.);
#7326=ORIENTED_EDGE('',*,*,#5106,.T.);
#7327=ORIENTED_EDGE('',*,*,#5107,.F.);
#7328=ORIENTED_EDGE('',*,*,#5108,.T.);
#7329=ORIENTED_EDGE('',*,*,#5109,.T.);
#7330=ORIENTED_EDGE('',*,*,#5110,.F.);
#7331=ORIENTED_EDGE('',*,*,#5111,.F.);
#7332=ORIENTED_EDGE('',*,*,#5112,.T.);
#7333=ORIENTED_EDGE('',*,*,#5107,.T.);
#7334=ORIENTED_EDGE('',*,*,#5113,.F.);
#7335=ORIENTED_EDGE('',*,*,#5114,.F.);
#7336=ORIENTED_EDGE('',*,*,#5115,.T.);
#7337=ORIENTED_EDGE('',*,*,#5111,.T.);
#7338=ORIENTED_EDGE('',*,*,#5116,.F.);
#7339=ORIENTED_EDGE('',*,*,#5117,.F.);
#7340=ORIENTED_EDGE('',*,*,#5118,.T.);
#7341=ORIENTED_EDGE('',*,*,#5114,.T.);
#7342=ORIENTED_EDGE('',*,*,#5119,.F.);
#7343=ORIENTED_EDGE('',*,*,#5120,.F.);
#7344=ORIENTED_EDGE('',*,*,#5121,.T.);
#7345=ORIENTED_EDGE('',*,*,#5117,.T.);
#7346=ORIENTED_EDGE('',*,*,#5122,.F.);
#7347=ORIENTED_EDGE('',*,*,#5123,.F.);
#7348=ORIENTED_EDGE('',*,*,#5124,.T.);
#7349=ORIENTED_EDGE('',*,*,#5120,.T.);
#7350=ORIENTED_EDGE('',*,*,#5125,.F.);
#7351=ORIENTED_EDGE('',*,*,#5126,.F.);
#7352=ORIENTED_EDGE('',*,*,#5127,.T.);
#7353=ORIENTED_EDGE('',*,*,#5123,.T.);
#7354=ORIENTED_EDGE('',*,*,#5128,.F.);
#7355=ORIENTED_EDGE('',*,*,#5129,.F.);
#7356=ORIENTED_EDGE('',*,*,#5130,.T.);
#7357=ORIENTED_EDGE('',*,*,#5126,.T.);
#7358=ORIENTED_EDGE('',*,*,#5131,.F.);
#7359=ORIENTED_EDGE('',*,*,#5132,.F.);
#7360=ORIENTED_EDGE('',*,*,#5133,.T.);
#7361=ORIENTED_EDGE('',*,*,#5129,.T.);
#7362=ORIENTED_EDGE('',*,*,#5134,.F.);
#7363=ORIENTED_EDGE('',*,*,#5135,.F.);
#7364=ORIENTED_EDGE('',*,*,#5136,.T.);
#7365=ORIENTED_EDGE('',*,*,#5132,.T.);
#7366=ORIENTED_EDGE('',*,*,#5137,.F.);
#7367=ORIENTED_EDGE('',*,*,#5138,.F.);
#7368=ORIENTED_EDGE('',*,*,#5139,.T.);
#7369=ORIENTED_EDGE('',*,*,#5135,.T.);
#7370=ORIENTED_EDGE('',*,*,#5140,.F.);
#7371=ORIENTED_EDGE('',*,*,#5141,.F.);
#7372=ORIENTED_EDGE('',*,*,#5142,.T.);
#7373=ORIENTED_EDGE('',*,*,#5138,.T.);
#7374=ORIENTED_EDGE('',*,*,#5143,.F.);
#7375=ORIENTED_EDGE('',*,*,#5144,.F.);
#7376=ORIENTED_EDGE('',*,*,#5145,.T.);
#7377=ORIENTED_EDGE('',*,*,#5141,.T.);
#7378=ORIENTED_EDGE('',*,*,#5146,.F.);
#7379=ORIENTED_EDGE('',*,*,#5147,.F.);
#7380=ORIENTED_EDGE('',*,*,#5148,.T.);
#7381=ORIENTED_EDGE('',*,*,#5144,.T.);
#7382=ORIENTED_EDGE('',*,*,#5149,.F.);
#7383=ORIENTED_EDGE('',*,*,#5150,.F.);
#7384=ORIENTED_EDGE('',*,*,#5151,.T.);
#7385=ORIENTED_EDGE('',*,*,#5147,.T.);
#7386=ORIENTED_EDGE('',*,*,#5152,.F.);
#7387=ORIENTED_EDGE('',*,*,#5153,.F.);
#7388=ORIENTED_EDGE('',*,*,#5154,.T.);
#7389=ORIENTED_EDGE('',*,*,#5150,.T.);
#7390=ORIENTED_EDGE('',*,*,#5155,.F.);
#7391=ORIENTED_EDGE('',*,*,#5156,.F.);
#7392=ORIENTED_EDGE('',*,*,#5157,.T.);
#7393=ORIENTED_EDGE('',*,*,#5153,.T.);
#7394=ORIENTED_EDGE('',*,*,#5158,.F.);
#7395=ORIENTED_EDGE('',*,*,#5159,.F.);
#7396=ORIENTED_EDGE('',*,*,#5160,.T.);
#7397=ORIENTED_EDGE('',*,*,#5156,.T.);
#7398=ORIENTED_EDGE('',*,*,#5161,.F.);
#7399=ORIENTED_EDGE('',*,*,#5162,.F.);
#7400=ORIENTED_EDGE('',*,*,#5163,.T.);
#7401=ORIENTED_EDGE('',*,*,#5159,.T.);
#7402=ORIENTED_EDGE('',*,*,#5164,.F.);
#7403=ORIENTED_EDGE('',*,*,#5165,.F.);
#7404=ORIENTED_EDGE('',*,*,#5109,.F.);
#7405=ORIENTED_EDGE('',*,*,#5166,.F.);
#7406=ORIENTED_EDGE('',*,*,#5167,.F.);
#7407=ORIENTED_EDGE('',*,*,#5168,.F.);
#7408=ORIENTED_EDGE('',*,*,#5169,.T.);
#7409=ORIENTED_EDGE('',*,*,#5170,.F.);
#7410=ORIENTED_EDGE('',*,*,#5169,.F.);
#7411=ORIENTED_EDGE('',*,*,#5166,.T.);
#7412=ORIENTED_EDGE('',*,*,#5108,.F.);
#7413=ORIENTED_EDGE('',*,*,#5112,.F.);
#7414=ORIENTED_EDGE('',*,*,#5115,.F.);
#7415=ORIENTED_EDGE('',*,*,#5118,.F.);
#7416=ORIENTED_EDGE('',*,*,#5121,.F.);
#7417=ORIENTED_EDGE('',*,*,#5124,.F.);
#7418=ORIENTED_EDGE('',*,*,#5127,.F.);
#7419=ORIENTED_EDGE('',*,*,#5130,.F.);
#7420=ORIENTED_EDGE('',*,*,#5133,.F.);
#7421=ORIENTED_EDGE('',*,*,#5136,.F.);
#7422=ORIENTED_EDGE('',*,*,#5139,.F.);
#7423=ORIENTED_EDGE('',*,*,#5142,.F.);
#7424=ORIENTED_EDGE('',*,*,#5145,.F.);
#7425=ORIENTED_EDGE('',*,*,#5148,.F.);
#7426=ORIENTED_EDGE('',*,*,#5151,.F.);
#7427=ORIENTED_EDGE('',*,*,#5154,.F.);
#7428=ORIENTED_EDGE('',*,*,#5157,.F.);
#7429=ORIENTED_EDGE('',*,*,#5160,.F.);
#7430=ORIENTED_EDGE('',*,*,#5163,.F.);
#7431=ORIENTED_EDGE('',*,*,#5171,.F.);
#7432=ORIENTED_EDGE('',*,*,#5172,.F.);
#7433=ORIENTED_EDGE('',*,*,#5050,.F.);
#7434=ORIENTED_EDGE('',*,*,#5054,.F.);
#7435=ORIENTED_EDGE('',*,*,#5057,.F.);
#7436=ORIENTED_EDGE('',*,*,#5060,.F.);
#7437=ORIENTED_EDGE('',*,*,#5063,.F.);
#7438=ORIENTED_EDGE('',*,*,#5066,.F.);
#7439=ORIENTED_EDGE('',*,*,#5069,.F.);
#7440=ORIENTED_EDGE('',*,*,#5072,.F.);
#7441=ORIENTED_EDGE('',*,*,#5075,.F.);
#7442=ORIENTED_EDGE('',*,*,#5078,.F.);
#7443=ORIENTED_EDGE('',*,*,#5081,.F.);
#7444=ORIENTED_EDGE('',*,*,#5084,.F.);
#7445=ORIENTED_EDGE('',*,*,#5087,.F.);
#7446=ORIENTED_EDGE('',*,*,#5090,.F.);
#7447=ORIENTED_EDGE('',*,*,#5093,.F.);
#7448=ORIENTED_EDGE('',*,*,#5096,.F.);
#7449=ORIENTED_EDGE('',*,*,#5099,.F.);
#7450=ORIENTED_EDGE('',*,*,#5102,.F.);
#7451=ORIENTED_EDGE('',*,*,#5105,.F.);
#7452=ORIENTED_EDGE('',*,*,#5173,.F.);
#7453=ORIENTED_EDGE('',*,*,#5162,.T.);
#7454=ORIENTED_EDGE('',*,*,#5174,.F.);
#7455=ORIENTED_EDGE('',*,*,#5175,.F.);
#7456=ORIENTED_EDGE('',*,*,#5171,.T.);
#7457=ORIENTED_EDGE('',*,*,#5165,.T.);
#7458=ORIENTED_EDGE('',*,*,#5168,.T.);
#7459=ORIENTED_EDGE('',*,*,#5176,.F.);
#7460=ORIENTED_EDGE('',*,*,#5106,.F.);
#7461=ORIENTED_EDGE('',*,*,#5103,.F.);
#7462=ORIENTED_EDGE('',*,*,#5100,.F.);
#7463=ORIENTED_EDGE('',*,*,#5097,.F.);
#7464=ORIENTED_EDGE('',*,*,#5094,.F.);
#7465=ORIENTED_EDGE('',*,*,#5091,.F.);
#7466=ORIENTED_EDGE('',*,*,#5088,.F.);
#7467=ORIENTED_EDGE('',*,*,#5085,.F.);
#7468=ORIENTED_EDGE('',*,*,#5082,.F.);
#7469=ORIENTED_EDGE('',*,*,#5079,.F.);
#7470=ORIENTED_EDGE('',*,*,#5076,.F.);
#7471=ORIENTED_EDGE('',*,*,#5073,.F.);
#7472=ORIENTED_EDGE('',*,*,#5070,.F.);
#7473=ORIENTED_EDGE('',*,*,#5067,.F.);
#7474=ORIENTED_EDGE('',*,*,#5064,.F.);
#7475=ORIENTED_EDGE('',*,*,#5061,.F.);
#7476=ORIENTED_EDGE('',*,*,#5058,.F.);
#7477=ORIENTED_EDGE('',*,*,#5055,.F.);
#7478=ORIENTED_EDGE('',*,*,#5052,.F.);
#7479=ORIENTED_EDGE('',*,*,#5177,.F.);
#7480=ORIENTED_EDGE('',*,*,#5174,.T.);
#7481=ORIENTED_EDGE('',*,*,#5164,.T.);
#7482=ORIENTED_EDGE('',*,*,#5161,.T.);
#7483=ORIENTED_EDGE('',*,*,#5158,.T.);
#7484=ORIENTED_EDGE('',*,*,#5155,.T.);
#7485=ORIENTED_EDGE('',*,*,#5152,.T.);
#7486=ORIENTED_EDGE('',*,*,#5149,.T.);
#7487=ORIENTED_EDGE('',*,*,#5146,.T.);
#7488=ORIENTED_EDGE('',*,*,#5143,.T.);
#7489=ORIENTED_EDGE('',*,*,#5140,.T.);
#7490=ORIENTED_EDGE('',*,*,#5137,.T.);
#7491=ORIENTED_EDGE('',*,*,#5134,.T.);
#7492=ORIENTED_EDGE('',*,*,#5131,.T.);
#7493=ORIENTED_EDGE('',*,*,#5128,.T.);
#7494=ORIENTED_EDGE('',*,*,#5125,.T.);
#7495=ORIENTED_EDGE('',*,*,#5122,.T.);
#7496=ORIENTED_EDGE('',*,*,#5119,.T.);
#7497=ORIENTED_EDGE('',*,*,#5116,.T.);
#7498=ORIENTED_EDGE('',*,*,#5113,.T.);
#7499=ORIENTED_EDGE('',*,*,#5110,.T.);
#7500=ORIENTED_EDGE('',*,*,#5104,.T.);
#7501=ORIENTED_EDGE('',*,*,#5176,.T.);
#7502=ORIENTED_EDGE('',*,*,#5167,.T.);
#7503=ORIENTED_EDGE('',*,*,#5173,.T.);
#7504=ORIENTED_EDGE('',*,*,#5178,.F.);
#7505=ORIENTED_EDGE('',*,*,#5179,.T.);
#7506=ORIENTED_EDGE('',*,*,#5180,.T.);
#7507=ORIENTED_EDGE('',*,*,#5181,.F.);
#7508=ORIENTED_EDGE('',*,*,#5182,.F.);
#7509=ORIENTED_EDGE('',*,*,#5183,.T.);
#7510=ORIENTED_EDGE('',*,*,#5184,.T.);
#7511=ORIENTED_EDGE('',*,*,#5179,.F.);
#7512=ORIENTED_EDGE('',*,*,#5185,.F.);
#7513=ORIENTED_EDGE('',*,*,#5186,.T.);
#7514=ORIENTED_EDGE('',*,*,#5187,.T.);
#7515=ORIENTED_EDGE('',*,*,#5183,.F.);
#7516=ORIENTED_EDGE('',*,*,#5188,.F.);
#7517=ORIENTED_EDGE('',*,*,#5189,.T.);
#7518=ORIENTED_EDGE('',*,*,#5190,.T.);
#7519=ORIENTED_EDGE('',*,*,#5186,.F.);
#7520=ORIENTED_EDGE('',*,*,#5191,.F.);
#7521=ORIENTED_EDGE('',*,*,#5192,.T.);
#7522=ORIENTED_EDGE('',*,*,#5193,.T.);
#7523=ORIENTED_EDGE('',*,*,#5189,.F.);
#7524=ORIENTED_EDGE('',*,*,#5194,.F.);
#7525=ORIENTED_EDGE('',*,*,#5181,.T.);
#7526=ORIENTED_EDGE('',*,*,#5195,.T.);
#7527=ORIENTED_EDGE('',*,*,#5192,.F.);
#7528=ORIENTED_EDGE('',*,*,#5195,.F.);
#7529=ORIENTED_EDGE('',*,*,#5180,.F.);
#7530=ORIENTED_EDGE('',*,*,#5184,.F.);
#7531=ORIENTED_EDGE('',*,*,#5187,.F.);
#7532=ORIENTED_EDGE('',*,*,#5190,.F.);
#7533=ORIENTED_EDGE('',*,*,#5193,.F.);
#7534=ORIENTED_EDGE('',*,*,#5196,.T.);
#7535=ORIENTED_EDGE('',*,*,#5172,.T.);
#7536=ORIENTED_EDGE('',*,*,#5175,.T.);
#7537=ORIENTED_EDGE('',*,*,#5177,.T.);
#7538=ORIENTED_EDGE('',*,*,#5051,.F.);
#7539=ORIENTED_EDGE('',*,*,#5196,.F.);
#7540=ORIENTED_EDGE('',*,*,#5197,.T.);
#7541=ORIENTED_EDGE('',*,*,#5198,.T.);
#7542=ORIENTED_EDGE('',*,*,#5197,.F.);
#7543=ORIENTED_EDGE('',*,*,#5198,.F.);
#7544=ORIENTED_EDGE('',*,*,#5178,.T.);
#7545=ORIENTED_EDGE('',*,*,#5194,.T.);
#7546=ORIENTED_EDGE('',*,*,#5191,.T.);
#7547=ORIENTED_EDGE('',*,*,#5188,.T.);
#7548=ORIENTED_EDGE('',*,*,#5185,.T.);
#7549=ORIENTED_EDGE('',*,*,#5182,.T.);
#7550=ORIENTED_EDGE('',*,*,#5170,.T.);
#7551=ORIENTED_EDGE('',*,*,#5199,.F.);
#7552=ORIENTED_EDGE('',*,*,#5200,.T.);
#7553=ORIENTED_EDGE('',*,*,#5201,.T.);
#7554=ORIENTED_EDGE('',*,*,#5202,.T.);
#7555=ORIENTED_EDGE('',*,*,#5203,.F.);
#7556=ORIENTED_EDGE('',*,*,#5204,.T.);
#7557=ORIENTED_EDGE('',*,*,#5199,.T.);
#7558=ORIENTED_EDGE('',*,*,#5205,.T.);
#7559=ORIENTED_EDGE('',*,*,#5206,.F.);
#7560=ORIENTED_EDGE('',*,*,#5207,.T.);
#7561=ORIENTED_EDGE('',*,*,#5203,.T.);
#7562=ORIENTED_EDGE('',*,*,#5208,.T.);
#7563=ORIENTED_EDGE('',*,*,#5209,.F.);
#7564=ORIENTED_EDGE('',*,*,#5210,.T.);
#7565=ORIENTED_EDGE('',*,*,#5206,.T.);
#7566=ORIENTED_EDGE('',*,*,#5211,.T.);
#7567=ORIENTED_EDGE('',*,*,#5212,.F.);
#7568=ORIENTED_EDGE('',*,*,#5213,.T.);
#7569=ORIENTED_EDGE('',*,*,#5209,.T.);
#7570=ORIENTED_EDGE('',*,*,#5214,.T.);
#7571=ORIENTED_EDGE('',*,*,#5215,.F.);
#7572=ORIENTED_EDGE('',*,*,#5216,.T.);
#7573=ORIENTED_EDGE('',*,*,#5212,.T.);
#7574=ORIENTED_EDGE('',*,*,#5217,.T.);
#7575=ORIENTED_EDGE('',*,*,#5218,.F.);
#7576=ORIENTED_EDGE('',*,*,#5219,.T.);
#7577=ORIENTED_EDGE('',*,*,#5215,.T.);
#7578=ORIENTED_EDGE('',*,*,#5220,.T.);
#7579=ORIENTED_EDGE('',*,*,#5221,.F.);
#7580=ORIENTED_EDGE('',*,*,#5222,.T.);
#7581=ORIENTED_EDGE('',*,*,#5218,.T.);
#7582=ORIENTED_EDGE('',*,*,#5223,.T.);
#7583=ORIENTED_EDGE('',*,*,#5224,.F.);
#7584=ORIENTED_EDGE('',*,*,#5225,.T.);
#7585=ORIENTED_EDGE('',*,*,#5221,.T.);
#7586=ORIENTED_EDGE('',*,*,#5226,.T.);
#7587=ORIENTED_EDGE('',*,*,#5227,.F.);
#7588=ORIENTED_EDGE('',*,*,#5228,.T.);
#7589=ORIENTED_EDGE('',*,*,#5224,.T.);
#7590=ORIENTED_EDGE('',*,*,#5229,.T.);
#7591=ORIENTED_EDGE('',*,*,#5230,.F.);
#7592=ORIENTED_EDGE('',*,*,#5231,.T.);
#7593=ORIENTED_EDGE('',*,*,#5227,.T.);
#7594=ORIENTED_EDGE('',*,*,#5232,.T.);
#7595=ORIENTED_EDGE('',*,*,#5233,.F.);
#7596=ORIENTED_EDGE('',*,*,#5234,.T.);
#7597=ORIENTED_EDGE('',*,*,#5235,.T.);
#7598=ORIENTED_EDGE('',*,*,#5236,.F.);
#7599=ORIENTED_EDGE('',*,*,#5237,.F.);
#7600=ORIENTED_EDGE('',*,*,#5238,.T.);
#7601=ORIENTED_EDGE('',*,*,#5233,.T.);
#7602=ORIENTED_EDGE('',*,*,#5239,.F.);
#7603=ORIENTED_EDGE('',*,*,#5240,.F.);
#7604=ORIENTED_EDGE('',*,*,#5241,.T.);
#7605=ORIENTED_EDGE('',*,*,#5237,.T.);
#7606=ORIENTED_EDGE('',*,*,#5242,.F.);
#7607=ORIENTED_EDGE('',*,*,#5243,.F.);
#7608=ORIENTED_EDGE('',*,*,#5244,.T.);
#7609=ORIENTED_EDGE('',*,*,#5240,.T.);
#7610=ORIENTED_EDGE('',*,*,#5245,.F.);
#7611=ORIENTED_EDGE('',*,*,#5246,.F.);
#7612=ORIENTED_EDGE('',*,*,#5247,.T.);
#7613=ORIENTED_EDGE('',*,*,#5243,.T.);
#7614=ORIENTED_EDGE('',*,*,#5248,.F.);
#7615=ORIENTED_EDGE('',*,*,#5249,.F.);
#7616=ORIENTED_EDGE('',*,*,#5250,.T.);
#7617=ORIENTED_EDGE('',*,*,#5246,.T.);
#7618=ORIENTED_EDGE('',*,*,#5251,.F.);
#7619=ORIENTED_EDGE('',*,*,#5252,.F.);
#7620=ORIENTED_EDGE('',*,*,#5253,.T.);
#7621=ORIENTED_EDGE('',*,*,#5249,.T.);
#7622=ORIENTED_EDGE('',*,*,#5254,.F.);
#7623=ORIENTED_EDGE('',*,*,#5255,.F.);
#7624=ORIENTED_EDGE('',*,*,#5256,.T.);
#7625=ORIENTED_EDGE('',*,*,#5252,.T.);
#7626=ORIENTED_EDGE('',*,*,#5257,.F.);
#7627=ORIENTED_EDGE('',*,*,#5258,.F.);
#7628=ORIENTED_EDGE('',*,*,#5259,.T.);
#7629=ORIENTED_EDGE('',*,*,#5255,.T.);
#7630=ORIENTED_EDGE('',*,*,#5260,.F.);
#7631=ORIENTED_EDGE('',*,*,#5261,.F.);
#7632=ORIENTED_EDGE('',*,*,#5262,.T.);
#7633=ORIENTED_EDGE('',*,*,#5258,.T.);
#7634=ORIENTED_EDGE('',*,*,#5263,.F.);
#7635=ORIENTED_EDGE('',*,*,#5264,.F.);
#7636=ORIENTED_EDGE('',*,*,#5265,.T.);
#7637=ORIENTED_EDGE('',*,*,#5261,.T.);
#7638=ORIENTED_EDGE('',*,*,#5266,.F.);
#7639=ORIENTED_EDGE('',*,*,#5267,.F.);
#7640=ORIENTED_EDGE('',*,*,#5235,.F.);
#7641=ORIENTED_EDGE('',*,*,#5268,.F.);
#7642=ORIENTED_EDGE('',*,*,#5269,.F.);
#7643=ORIENTED_EDGE('',*,*,#5270,.F.);
#7644=ORIENTED_EDGE('',*,*,#5271,.T.);
#7645=ORIENTED_EDGE('',*,*,#5272,.F.);
#7646=ORIENTED_EDGE('',*,*,#5271,.F.);
#7647=ORIENTED_EDGE('',*,*,#5268,.T.);
#7648=ORIENTED_EDGE('',*,*,#5234,.F.);
#7649=ORIENTED_EDGE('',*,*,#5238,.F.);
#7650=ORIENTED_EDGE('',*,*,#5241,.F.);
#7651=ORIENTED_EDGE('',*,*,#5244,.F.);
#7652=ORIENTED_EDGE('',*,*,#5247,.F.);
#7653=ORIENTED_EDGE('',*,*,#5250,.F.);
#7654=ORIENTED_EDGE('',*,*,#5253,.F.);
#7655=ORIENTED_EDGE('',*,*,#5256,.F.);
#7656=ORIENTED_EDGE('',*,*,#5259,.F.);
#7657=ORIENTED_EDGE('',*,*,#5262,.F.);
#7658=ORIENTED_EDGE('',*,*,#5265,.F.);
#7659=ORIENTED_EDGE('',*,*,#5273,.F.);
#7660=ORIENTED_EDGE('',*,*,#5274,.F.);
#7661=ORIENTED_EDGE('',*,*,#5200,.F.);
#7662=ORIENTED_EDGE('',*,*,#5204,.F.);
#7663=ORIENTED_EDGE('',*,*,#5207,.F.);
#7664=ORIENTED_EDGE('',*,*,#5210,.F.);
#7665=ORIENTED_EDGE('',*,*,#5213,.F.);
#7666=ORIENTED_EDGE('',*,*,#5216,.F.);
#7667=ORIENTED_EDGE('',*,*,#5219,.F.);
#7668=ORIENTED_EDGE('',*,*,#5222,.F.);
#7669=ORIENTED_EDGE('',*,*,#5225,.F.);
#7670=ORIENTED_EDGE('',*,*,#5228,.F.);
#7671=ORIENTED_EDGE('',*,*,#5231,.F.);
#7672=ORIENTED_EDGE('',*,*,#5275,.F.);
#7673=ORIENTED_EDGE('',*,*,#5264,.T.);
#7674=ORIENTED_EDGE('',*,*,#5276,.F.);
#7675=ORIENTED_EDGE('',*,*,#5277,.F.);
#7676=ORIENTED_EDGE('',*,*,#5273,.T.);
#7677=ORIENTED_EDGE('',*,*,#5267,.T.);
#7678=ORIENTED_EDGE('',*,*,#5270,.T.);
#7679=ORIENTED_EDGE('',*,*,#5278,.F.);
#7680=ORIENTED_EDGE('',*,*,#5232,.F.);
#7681=ORIENTED_EDGE('',*,*,#5229,.F.);
#7682=ORIENTED_EDGE('',*,*,#5226,.F.);
#7683=ORIENTED_EDGE('',*,*,#5223,.F.);
#7684=ORIENTED_EDGE('',*,*,#5220,.F.);
#7685=ORIENTED_EDGE('',*,*,#5217,.F.);
#7686=ORIENTED_EDGE('',*,*,#5214,.F.);
#7687=ORIENTED_EDGE('',*,*,#5211,.F.);
#7688=ORIENTED_EDGE('',*,*,#5208,.F.);
#7689=ORIENTED_EDGE('',*,*,#5205,.F.);
#7690=ORIENTED_EDGE('',*,*,#5202,.F.);
#7691=ORIENTED_EDGE('',*,*,#5279,.F.);
#7692=ORIENTED_EDGE('',*,*,#5276,.T.);
#7693=ORIENTED_EDGE('',*,*,#5266,.T.);
#7694=ORIENTED_EDGE('',*,*,#5263,.T.);
#7695=ORIENTED_EDGE('',*,*,#5260,.T.);
#7696=ORIENTED_EDGE('',*,*,#5257,.T.);
#7697=ORIENTED_EDGE('',*,*,#5254,.T.);
#7698=ORIENTED_EDGE('',*,*,#5251,.T.);
#7699=ORIENTED_EDGE('',*,*,#5248,.T.);
#7700=ORIENTED_EDGE('',*,*,#5245,.T.);
#7701=ORIENTED_EDGE('',*,*,#5242,.T.);
#7702=ORIENTED_EDGE('',*,*,#5239,.T.);
#7703=ORIENTED_EDGE('',*,*,#5236,.T.);
#7704=ORIENTED_EDGE('',*,*,#5230,.T.);
#7705=ORIENTED_EDGE('',*,*,#5278,.T.);
#7706=ORIENTED_EDGE('',*,*,#5269,.T.);
#7707=ORIENTED_EDGE('',*,*,#5275,.T.);
#7708=ORIENTED_EDGE('',*,*,#5280,.F.);
#7709=ORIENTED_EDGE('',*,*,#5281,.T.);
#7710=ORIENTED_EDGE('',*,*,#5282,.T.);
#7711=ORIENTED_EDGE('',*,*,#5283,.F.);
#7712=ORIENTED_EDGE('',*,*,#5284,.F.);
#7713=ORIENTED_EDGE('',*,*,#5285,.T.);
#7714=ORIENTED_EDGE('',*,*,#5286,.T.);
#7715=ORIENTED_EDGE('',*,*,#5281,.F.);
#7716=ORIENTED_EDGE('',*,*,#5287,.F.);
#7717=ORIENTED_EDGE('',*,*,#5288,.T.);
#7718=ORIENTED_EDGE('',*,*,#5289,.T.);
#7719=ORIENTED_EDGE('',*,*,#5285,.F.);
#7720=ORIENTED_EDGE('',*,*,#5290,.F.);
#7721=ORIENTED_EDGE('',*,*,#5291,.T.);
#7722=ORIENTED_EDGE('',*,*,#5292,.T.);
#7723=ORIENTED_EDGE('',*,*,#5288,.F.);
#7724=ORIENTED_EDGE('',*,*,#5293,.F.);
#7725=ORIENTED_EDGE('',*,*,#5294,.T.);
#7726=ORIENTED_EDGE('',*,*,#5295,.T.);
#7727=ORIENTED_EDGE('',*,*,#5291,.F.);
#7728=ORIENTED_EDGE('',*,*,#5296,.F.);
#7729=ORIENTED_EDGE('',*,*,#5283,.T.);
#7730=ORIENTED_EDGE('',*,*,#5297,.T.);
#7731=ORIENTED_EDGE('',*,*,#5294,.F.);
#7732=ORIENTED_EDGE('',*,*,#5297,.F.);
#7733=ORIENTED_EDGE('',*,*,#5282,.F.);
#7734=ORIENTED_EDGE('',*,*,#5286,.F.);
#7735=ORIENTED_EDGE('',*,*,#5289,.F.);
#7736=ORIENTED_EDGE('',*,*,#5292,.F.);
#7737=ORIENTED_EDGE('',*,*,#5295,.F.);
#7738=ORIENTED_EDGE('',*,*,#5298,.T.);
#7739=ORIENTED_EDGE('',*,*,#5274,.T.);
#7740=ORIENTED_EDGE('',*,*,#5277,.T.);
#7741=ORIENTED_EDGE('',*,*,#5279,.T.);
#7742=ORIENTED_EDGE('',*,*,#5201,.F.);
#7743=ORIENTED_EDGE('',*,*,#5298,.F.);
#7744=ORIENTED_EDGE('',*,*,#5299,.T.);
#7745=ORIENTED_EDGE('',*,*,#5300,.T.);
#7746=ORIENTED_EDGE('',*,*,#5299,.F.);
#7747=ORIENTED_EDGE('',*,*,#5300,.F.);
#7748=ORIENTED_EDGE('',*,*,#5280,.T.);
#7749=ORIENTED_EDGE('',*,*,#5296,.T.);
#7750=ORIENTED_EDGE('',*,*,#5293,.T.);
#7751=ORIENTED_EDGE('',*,*,#5290,.T.);
#7752=ORIENTED_EDGE('',*,*,#5287,.T.);
#7753=ORIENTED_EDGE('',*,*,#5284,.T.);
#7754=ORIENTED_EDGE('',*,*,#5272,.T.);
#7755=ORIENTED_EDGE('',*,*,#5301,.F.);
#7756=ORIENTED_EDGE('',*,*,#5302,.T.);
#7757=ORIENTED_EDGE('',*,*,#5303,.T.);
#7758=ORIENTED_EDGE('',*,*,#5302,.F.);
#7759=ORIENTED_EDGE('',*,*,#5304,.F.);
#7760=ORIENTED_EDGE('',*,*,#5305,.T.);
#7761=ORIENTED_EDGE('',*,*,#5306,.T.);
#7762=ORIENTED_EDGE('',*,*,#5305,.F.);
#7763=ORIENTED_EDGE('',*,*,#5304,.T.);
#7764=ORIENTED_EDGE('',*,*,#5301,.T.);
#7765=ORIENTED_EDGE('',*,*,#5306,.F.);
#7766=ORIENTED_EDGE('',*,*,#5303,.F.);
#7767=ORIENTED_EDGE('',*,*,#5307,.T.);
#7768=ORIENTED_EDGE('',*,*,#5308,.T.);
#7769=ORIENTED_EDGE('',*,*,#5309,.F.);
#7770=ORIENTED_EDGE('',*,*,#5310,.T.);
#7771=ORIENTED_EDGE('',*,*,#5311,.T.);
#7772=ORIENTED_EDGE('',*,*,#5312,.T.);
#7773=ORIENTED_EDGE('',*,*,#5307,.F.);
#7774=ORIENTED_EDGE('',*,*,#5313,.T.);
#7775=ORIENTED_EDGE('',*,*,#5314,.T.);
#7776=ORIENTED_EDGE('',*,*,#5315,.T.);
#7777=ORIENTED_EDGE('',*,*,#5311,.F.);
#7778=ORIENTED_EDGE('',*,*,#5316,.T.);
#7779=ORIENTED_EDGE('',*,*,#5317,.T.);
#7780=ORIENTED_EDGE('',*,*,#5318,.T.);
#7781=ORIENTED_EDGE('',*,*,#5314,.F.);
#7782=ORIENTED_EDGE('',*,*,#5319,.T.);
#7783=ORIENTED_EDGE('',*,*,#5320,.F.);
#7784=ORIENTED_EDGE('',*,*,#5321,.T.);
#7785=ORIENTED_EDGE('',*,*,#5322,.F.);
#7786=ORIENTED_EDGE('',*,*,#5323,.T.);
#7787=ORIENTED_EDGE('',*,*,#5324,.T.);
#7788=ORIENTED_EDGE('',*,*,#5325,.T.);
#7789=ORIENTED_EDGE('',*,*,#5326,.F.);
#7790=ORIENTED_EDGE('',*,*,#5327,.F.);
#7791=ORIENTED_EDGE('',*,*,#5328,.T.);
#7792=ORIENTED_EDGE('',*,*,#5329,.T.);
#7793=ORIENTED_EDGE('',*,*,#5324,.F.);
#7794=ORIENTED_EDGE('',*,*,#5330,.F.);
#7795=ORIENTED_EDGE('',*,*,#5331,.T.);
#7796=ORIENTED_EDGE('',*,*,#5332,.T.);
#7797=ORIENTED_EDGE('',*,*,#5328,.F.);
#7798=ORIENTED_EDGE('',*,*,#5333,.F.);
#7799=ORIENTED_EDGE('',*,*,#5334,.T.);
#7800=ORIENTED_EDGE('',*,*,#5335,.T.);
#7801=ORIENTED_EDGE('',*,*,#5331,.F.);
#7802=ORIENTED_EDGE('',*,*,#5336,.F.);
#7803=ORIENTED_EDGE('',*,*,#5337,.F.);
#7804=ORIENTED_EDGE('',*,*,#5338,.F.);
#7805=ORIENTED_EDGE('',*,*,#5339,.F.);
#7806=ORIENTED_EDGE('',*,*,#5340,.T.);
#7807=ORIENTED_EDGE('',*,*,#5337,.T.);
#7808=ORIENTED_EDGE('',*,*,#5341,.T.);
#7809=ORIENTED_EDGE('',*,*,#5334,.F.);
#7810=ORIENTED_EDGE('',*,*,#5342,.F.);
#7811=ORIENTED_EDGE('',*,*,#5343,.F.);
#7812=ORIENTED_EDGE('',*,*,#5325,.F.);
#7813=ORIENTED_EDGE('',*,*,#5329,.F.);
#7814=ORIENTED_EDGE('',*,*,#5332,.F.);
#7815=ORIENTED_EDGE('',*,*,#5335,.F.);
#7816=ORIENTED_EDGE('',*,*,#5341,.F.);
#7817=ORIENTED_EDGE('',*,*,#5340,.F.);
#7818=ORIENTED_EDGE('',*,*,#5344,.F.);
#7819=ORIENTED_EDGE('',*,*,#5321,.F.);
#7820=ORIENTED_EDGE('',*,*,#5345,.F.);
#7821=ORIENTED_EDGE('',*,*,#5319,.F.);
#7822=ORIENTED_EDGE('',*,*,#5316,.F.);
#7823=ORIENTED_EDGE('',*,*,#5313,.F.);
#7824=ORIENTED_EDGE('',*,*,#5310,.F.);
#7825=ORIENTED_EDGE('',*,*,#5346,.F.);
#7826=ORIENTED_EDGE('',*,*,#5308,.F.);
#7827=ORIENTED_EDGE('',*,*,#5312,.F.);
#7828=ORIENTED_EDGE('',*,*,#5315,.F.);
#7829=ORIENTED_EDGE('',*,*,#5318,.F.);
#7830=ORIENTED_EDGE('',*,*,#5347,.F.);
#7831=ORIENTED_EDGE('',*,*,#5323,.F.);
#7832=ORIENTED_EDGE('',*,*,#5348,.F.);
#7833=ORIENTED_EDGE('',*,*,#5338,.T.);
#7834=ORIENTED_EDGE('',*,*,#5342,.T.);
#7835=ORIENTED_EDGE('',*,*,#5336,.T.);
#7836=ORIENTED_EDGE('',*,*,#5333,.T.);
#7837=ORIENTED_EDGE('',*,*,#5330,.T.);
#7838=ORIENTED_EDGE('',*,*,#5327,.T.);
#7839=ORIENTED_EDGE('',*,*,#5349,.T.);
#7840=ORIENTED_EDGE('',*,*,#5350,.T.);
#7841=ORIENTED_EDGE('',*,*,#5351,.T.);
#7842=ORIENTED_EDGE('',*,*,#5352,.T.);
#7843=ORIENTED_EDGE('',*,*,#5353,.T.);
#7844=ORIENTED_EDGE('',*,*,#5354,.T.);
#7845=ORIENTED_EDGE('',*,*,#5344,.T.);
#7846=ORIENTED_EDGE('',*,*,#5339,.T.);
#7847=ORIENTED_EDGE('',*,*,#5348,.T.);
#7848=ORIENTED_EDGE('',*,*,#5322,.T.);
#7849=ORIENTED_EDGE('',*,*,#5320,.T.);
#7850=ORIENTED_EDGE('',*,*,#5347,.T.);
#7851=ORIENTED_EDGE('',*,*,#5317,.F.);
#7852=ORIENTED_EDGE('',*,*,#5345,.T.);
#7853=ORIENTED_EDGE('',*,*,#5355,.T.);
#7854=ORIENTED_EDGE('',*,*,#5356,.T.);
#7855=ORIENTED_EDGE('',*,*,#5354,.F.);
#7856=ORIENTED_EDGE('',*,*,#5357,.F.);
#7857=ORIENTED_EDGE('',*,*,#5358,.T.);
#7858=ORIENTED_EDGE('',*,*,#5357,.T.);
#7859=ORIENTED_EDGE('',*,*,#5353,.F.);
#7860=ORIENTED_EDGE('',*,*,#5359,.F.);
#7861=ORIENTED_EDGE('',*,*,#5360,.T.);
#7862=ORIENTED_EDGE('',*,*,#5359,.T.);
#7863=ORIENTED_EDGE('',*,*,#5352,.F.);
#7864=ORIENTED_EDGE('',*,*,#5361,.F.);
#7865=ORIENTED_EDGE('',*,*,#5362,.T.);
#7866=ORIENTED_EDGE('',*,*,#5361,.T.);
#7867=ORIENTED_EDGE('',*,*,#5351,.F.);
#7868=ORIENTED_EDGE('',*,*,#5363,.F.);
#7869=ORIENTED_EDGE('',*,*,#5364,.T.);
#7870=ORIENTED_EDGE('',*,*,#5363,.T.);
#7871=ORIENTED_EDGE('',*,*,#5350,.F.);
#7872=ORIENTED_EDGE('',*,*,#5365,.F.);
#7873=ORIENTED_EDGE('',*,*,#5366,.T.);
#7874=ORIENTED_EDGE('',*,*,#5365,.T.);
#7875=ORIENTED_EDGE('',*,*,#5349,.F.);
#7876=ORIENTED_EDGE('',*,*,#5356,.F.);
#7877=ORIENTED_EDGE('',*,*,#5366,.F.);
#7878=ORIENTED_EDGE('',*,*,#5355,.F.);
#7879=ORIENTED_EDGE('',*,*,#5358,.F.);
#7880=ORIENTED_EDGE('',*,*,#5360,.F.);
#7881=ORIENTED_EDGE('',*,*,#5362,.F.);
#7882=ORIENTED_EDGE('',*,*,#5364,.F.);
#7883=ORIENTED_EDGE('',*,*,#5343,.T.);
#7884=ORIENTED_EDGE('',*,*,#5309,.T.);
#7885=ORIENTED_EDGE('',*,*,#5346,.T.);
#7886=ORIENTED_EDGE('',*,*,#5326,.T.);
#7887=CYLINDRICAL_SURFACE('',#8894,2.5175);
#7888=CYLINDRICAL_SURFACE('',#8898,2.5175);
#7889=CYLINDRICAL_SURFACE('',#8899,2.5175);
#7890=CYLINDRICAL_SURFACE('',#8900,2.5175);
#7891=CYLINDRICAL_SURFACE('',#8901,2.5175);
#7892=CYLINDRICAL_SURFACE('',#8902,2.5175);
#7893=CYLINDRICAL_SURFACE('',#8903,2.5175);
#7894=CYLINDRICAL_SURFACE('',#8904,2.5175);
#7895=CYLINDRICAL_SURFACE('',#8905,2.5175);
#7896=CYLINDRICAL_SURFACE('',#8906,2.5175);
#7897=CYLINDRICAL_SURFACE('',#8907,2.5175);
#7898=CYLINDRICAL_SURFACE('',#8908,2.5175);
#7899=CYLINDRICAL_SURFACE('',#8909,2.5175);
#7900=CYLINDRICAL_SURFACE('',#8910,2.5175);
#7901=CYLINDRICAL_SURFACE('',#8911,2.5175);
#7902=CYLINDRICAL_SURFACE('',#8912,2.5175);
#7903=CYLINDRICAL_SURFACE('',#8913,2.5175);
#7904=CYLINDRICAL_SURFACE('',#8915,3.0735);
#7905=CYLINDRICAL_SURFACE('',#8917,3.0735);
#7906=CYLINDRICAL_SURFACE('',#8918,3.0735);
#7907=CYLINDRICAL_SURFACE('',#8919,3.0735);
#7908=CYLINDRICAL_SURFACE('',#8920,3.0735);
#7909=CYLINDRICAL_SURFACE('',#8921,3.0735);
#7910=CYLINDRICAL_SURFACE('',#8922,3.0735);
#7911=CYLINDRICAL_SURFACE('',#8923,3.0735);
#7912=CYLINDRICAL_SURFACE('',#8924,3.0735);
#7913=CYLINDRICAL_SURFACE('',#8925,3.0735);
#7914=CYLINDRICAL_SURFACE('',#8926,3.0735);
#7915=CYLINDRICAL_SURFACE('',#8927,3.0735);
#7916=CYLINDRICAL_SURFACE('',#8928,3.0735);
#7917=CYLINDRICAL_SURFACE('',#8929,3.0735);
#7918=CYLINDRICAL_SURFACE('',#8930,3.0735);
#7919=CYLINDRICAL_SURFACE('',#8931,3.0735);
#7920=CYLINDRICAL_SURFACE('',#8932,3.0735);
#7921=CYLINDRICAL_SURFACE('',#8934,2.5175);
#7922=CYLINDRICAL_SURFACE('',#8938,2.5175);
#7923=CYLINDRICAL_SURFACE('',#8939,2.5175);
#7924=CYLINDRICAL_SURFACE('',#8940,2.5175);
#7925=CYLINDRICAL_SURFACE('',#8941,2.5175);
#7926=CYLINDRICAL_SURFACE('',#8942,2.5175);
#7927=CYLINDRICAL_SURFACE('',#8943,2.5175);
#7928=CYLINDRICAL_SURFACE('',#8944,2.5175);
#7929=CYLINDRICAL_SURFACE('',#8945,2.5175);
#7930=CYLINDRICAL_SURFACE('',#8946,2.5175);
#7931=CYLINDRICAL_SURFACE('',#8947,2.5175);
#7932=CYLINDRICAL_SURFACE('',#8948,2.5175);
#7933=CYLINDRICAL_SURFACE('',#8949,2.5175);
#7934=CYLINDRICAL_SURFACE('',#8950,2.5175);
#7935=CYLINDRICAL_SURFACE('',#8951,2.5175);
#7936=CYLINDRICAL_SURFACE('',#8952,2.5175);
#7937=CYLINDRICAL_SURFACE('',#8953,2.5175);
#7938=CYLINDRICAL_SURFACE('',#8955,3.0735);
#7939=CYLINDRICAL_SURFACE('',#8957,3.0735);
#7940=CYLINDRICAL_SURFACE('',#8958,3.0735);
#7941=CYLINDRICAL_SURFACE('',#8959,3.0735);
#7942=CYLINDRICAL_SURFACE('',#8960,3.0735);
#7943=CYLINDRICAL_SURFACE('',#8961,3.0735);
#7944=CYLINDRICAL_SURFACE('',#8962,3.0735);
#7945=CYLINDRICAL_SURFACE('',#8963,3.0735);
#7946=CYLINDRICAL_SURFACE('',#8964,3.0735);
#7947=CYLINDRICAL_SURFACE('',#8965,3.0735);
#7948=CYLINDRICAL_SURFACE('',#8966,3.0735);
#7949=CYLINDRICAL_SURFACE('',#8967,3.0735);
#7950=CYLINDRICAL_SURFACE('',#8968,3.0735);
#7951=CYLINDRICAL_SURFACE('',#8969,3.0735);
#7952=CYLINDRICAL_SURFACE('',#8970,3.0735);
#7953=CYLINDRICAL_SURFACE('',#8971,3.0735);
#7954=CYLINDRICAL_SURFACE('',#8972,3.0735);
#7955=CYLINDRICAL_SURFACE('',#8974,2.5175);
#7956=CYLINDRICAL_SURFACE('',#8978,2.5175);
#7957=CYLINDRICAL_SURFACE('',#8979,2.5175);
#7958=CYLINDRICAL_SURFACE('',#8980,2.5175);
#7959=CYLINDRICAL_SURFACE('',#8981,2.5175);
#7960=CYLINDRICAL_SURFACE('',#8982,2.5175);
#7961=CYLINDRICAL_SURFACE('',#8983,2.5175);
#7962=CYLINDRICAL_SURFACE('',#8984,2.5175);
#7963=CYLINDRICAL_SURFACE('',#8985,2.5175);
#7964=CYLINDRICAL_SURFACE('',#8986,2.5175);
#7965=CYLINDRICAL_SURFACE('',#8987,2.5175);
#7966=CYLINDRICAL_SURFACE('',#8988,2.5175);
#7967=CYLINDRICAL_SURFACE('',#8989,2.5175);
#7968=CYLINDRICAL_SURFACE('',#8990,2.5175);
#7969=CYLINDRICAL_SURFACE('',#8991,2.5175);
#7970=CYLINDRICAL_SURFACE('',#8992,2.5175);
#7971=CYLINDRICAL_SURFACE('',#8993,2.5175);
#7972=CYLINDRICAL_SURFACE('',#8995,3.07349999999996);
#7973=CYLINDRICAL_SURFACE('',#8997,3.07349999999996);
#7974=CYLINDRICAL_SURFACE('',#8998,3.07349999999996);
#7975=CYLINDRICAL_SURFACE('',#8999,3.07349999999996);
#7976=CYLINDRICAL_SURFACE('',#9000,3.07349999999996);
#7977=CYLINDRICAL_SURFACE('',#9001,3.07349999999996);
#7978=CYLINDRICAL_SURFACE('',#9002,3.07349999999996);
#7979=CYLINDRICAL_SURFACE('',#9003,3.07349999999996);
#7980=CYLINDRICAL_SURFACE('',#9004,3.07349999999996);
#7981=CYLINDRICAL_SURFACE('',#9005,3.07349999999996);
#7982=CYLINDRICAL_SURFACE('',#9006,3.07349999999996);
#7983=CYLINDRICAL_SURFACE('',#9007,3.07349999999996);
#7984=CYLINDRICAL_SURFACE('',#9008,3.07349999999996);
#7985=CYLINDRICAL_SURFACE('',#9009,3.07349999999996);
#7986=CYLINDRICAL_SURFACE('',#9010,3.07349999999996);
#7987=CYLINDRICAL_SURFACE('',#9011,3.07349999999996);
#7988=CYLINDRICAL_SURFACE('',#9012,3.07349999999996);
#7989=CYLINDRICAL_SURFACE('',#9014,2.5175);
#7990=CYLINDRICAL_SURFACE('',#9018,2.5175);
#7991=CYLINDRICAL_SURFACE('',#9019,2.5175);
#7992=CYLINDRICAL_SURFACE('',#9020,2.5175);
#7993=CYLINDRICAL_SURFACE('',#9021,2.5175);
#7994=CYLINDRICAL_SURFACE('',#9022,2.5175);
#7995=CYLINDRICAL_SURFACE('',#9023,2.5175);
#7996=CYLINDRICAL_SURFACE('',#9024,2.5175);
#7997=CYLINDRICAL_SURFACE('',#9025,2.5175);
#7998=CYLINDRICAL_SURFACE('',#9026,2.5175);
#7999=CYLINDRICAL_SURFACE('',#9027,2.5175);
#8000=CYLINDRICAL_SURFACE('',#9028,2.5175);
#8001=CYLINDRICAL_SURFACE('',#9029,2.5175);
#8002=CYLINDRICAL_SURFACE('',#9030,2.5175);
#8003=CYLINDRICAL_SURFACE('',#9031,2.5175);
#8004=CYLINDRICAL_SURFACE('',#9032,2.5175);
#8005=CYLINDRICAL_SURFACE('',#9033,2.5175);
#8006=CYLINDRICAL_SURFACE('',#9035,3.07350000000003);
#8007=CYLINDRICAL_SURFACE('',#9037,3.07350000000003);
#8008=CYLINDRICAL_SURFACE('',#9038,3.07350000000003);
#8009=CYLINDRICAL_SURFACE('',#9039,3.07350000000003);
#8010=CYLINDRICAL_SURFACE('',#9040,3.07350000000003);
#8011=CYLINDRICAL_SURFACE('',#9041,3.07350000000003);
#8012=CYLINDRICAL_SURFACE('',#9042,3.07350000000003);
#8013=CYLINDRICAL_SURFACE('',#9043,3.07350000000003);
#8014=CYLINDRICAL_SURFACE('',#9044,3.07350000000003);
#8015=CYLINDRICAL_SURFACE('',#9045,3.07350000000003);
#8016=CYLINDRICAL_SURFACE('',#9046,3.07350000000003);
#8017=CYLINDRICAL_SURFACE('',#9047,3.07350000000003);
#8018=CYLINDRICAL_SURFACE('',#9048,3.07350000000003);
#8019=CYLINDRICAL_SURFACE('',#9049,3.07350000000003);
#8020=CYLINDRICAL_SURFACE('',#9050,3.07350000000003);
#8021=CYLINDRICAL_SURFACE('',#9051,3.07350000000003);
#8022=CYLINDRICAL_SURFACE('',#9052,3.07350000000003);
#8023=CYLINDRICAL_SURFACE('',#9055,3.07350000000003);
#8024=CYLINDRICAL_SURFACE('',#9056,2.5175);
#8025=CYLINDRICAL_SURFACE('',#9058,3.07349999999996);
#8026=CYLINDRICAL_SURFACE('',#9059,2.5175);
#8027=CYLINDRICAL_SURFACE('',#9061,3.0735);
#8028=CYLINDRICAL_SURFACE('',#9062,2.5175);
#8029=CYLINDRICAL_SURFACE('',#9064,3.0735);
#8030=CYLINDRICAL_SURFACE('',#9065,2.5175);
#8031=CYLINDRICAL_SURFACE('',#9081,4.5);
#8032=CYLINDRICAL_SURFACE('',#9084,3.5);
#8033=CYLINDRICAL_SURFACE('',#9087,3.5);
#8034=CYLINDRICAL_SURFACE('',#9090,3.5);
#8035=CYLINDRICAL_SURFACE('',#9093,3.5);
#8036=CYLINDRICAL_SURFACE('',#9114,1.666);
#8037=CYLINDRICAL_SURFACE('',#9117,1.666);
#8038=CYLINDRICAL_SURFACE('',#9118,1.666);
#8039=CYLINDRICAL_SURFACE('',#9119,1.666);
#8040=CYLINDRICAL_SURFACE('',#9120,1.666);
#8041=CYLINDRICAL_SURFACE('',#9121,1.666);
#8042=CYLINDRICAL_SURFACE('',#9122,1.666);
#8043=CYLINDRICAL_SURFACE('',#9123,1.666);
#8044=CYLINDRICAL_SURFACE('',#9124,1.666);
#8045=CYLINDRICAL_SURFACE('',#9125,1.666);
#8046=CYLINDRICAL_SURFACE('',#9126,1.666);
#8047=CYLINDRICAL_SURFACE('',#9127,1.666);
#8048=CYLINDRICAL_SURFACE('',#9128,1.666);
#8049=CYLINDRICAL_SURFACE('',#9129,1.666);
#8050=CYLINDRICAL_SURFACE('',#9130,1.666);
#8051=CYLINDRICAL_SURFACE('',#9132,2.05475);
#8052=CYLINDRICAL_SURFACE('',#9134,2.05475);
#8053=CYLINDRICAL_SURFACE('',#9135,2.05475);
#8054=CYLINDRICAL_SURFACE('',#9136,2.05475);
#8055=CYLINDRICAL_SURFACE('',#9137,2.05475);
#8056=CYLINDRICAL_SURFACE('',#9138,2.05475);
#8057=CYLINDRICAL_SURFACE('',#9139,2.05475);
#8058=CYLINDRICAL_SURFACE('',#9140,2.05475);
#8059=CYLINDRICAL_SURFACE('',#9141,2.05475);
#8060=CYLINDRICAL_SURFACE('',#9142,2.05475);
#8061=CYLINDRICAL_SURFACE('',#9143,2.05475);
#8062=CYLINDRICAL_SURFACE('',#9144,2.05475);
#8063=CYLINDRICAL_SURFACE('',#9145,2.05475);
#8064=CYLINDRICAL_SURFACE('',#9146,2.05475);
#8065=CYLINDRICAL_SURFACE('',#9147,2.05475);
#8066=CYLINDRICAL_SURFACE('',#9148,2.05475);
#8067=CYLINDRICAL_SURFACE('',#9151,2.05475);
#8068=CYLINDRICAL_SURFACE('',#9152,1.666);
#8069=CYLINDRICAL_SURFACE('',#9159,3.);
#8070=CYLINDRICAL_SURFACE('',#9166,4.);
#8071=CYLINDRICAL_SURFACE('',#9178,10.);
#8072=CYLINDRICAL_SURFACE('',#9181,4.);
#8073=CYLINDRICAL_SURFACE('',#9197,4.);
#8074=CYLINDRICAL_SURFACE('',#9200,8.);
#8075=CYLINDRICAL_SURFACE('',#9211,3.);
#8076=CYLINDRICAL_SURFACE('',#9213,6.);
#8077=CYLINDRICAL_SURFACE('',#9217,2.5);
#8078=CYLINDRICAL_SURFACE('',#9220,4.5);
#8079=CYLINDRICAL_SURFACE('',#9226,1.954);
#8080=CYLINDRICAL_SURFACE('',#9228,1.954);
#8081=CYLINDRICAL_SURFACE('',#9229,1.954);
#8082=CYLINDRICAL_SURFACE('',#9230,1.954);
#8083=CYLINDRICAL_SURFACE('',#9231,1.954);
#8084=CYLINDRICAL_SURFACE('',#9232,1.954);
#8085=CYLINDRICAL_SURFACE('',#9233,1.954);
#8086=CYLINDRICAL_SURFACE('',#9234,1.954);
#8087=CYLINDRICAL_SURFACE('',#9235,1.954);
#8088=CYLINDRICAL_SURFACE('',#9236,1.954);
#8089=CYLINDRICAL_SURFACE('',#9237,1.5555);
#8090=CYLINDRICAL_SURFACE('',#9239,1.5555);
#8091=CYLINDRICAL_SURFACE('',#9240,1.5555);
#8092=CYLINDRICAL_SURFACE('',#9241,1.5555);
#8093=CYLINDRICAL_SURFACE('',#9242,1.5555);
#8094=CYLINDRICAL_SURFACE('',#9243,1.5555);
#8095=CYLINDRICAL_SURFACE('',#9244,1.5555);
#8096=CYLINDRICAL_SURFACE('',#9245,1.5555);
#8097=CYLINDRICAL_SURFACE('',#9246,1.5555);
#8098=CYLINDRICAL_SURFACE('',#9247,1.5555);
#8099=CYLINDRICAL_SURFACE('',#9251,1.5555);
#8100=CYLINDRICAL_SURFACE('',#9253,1.954);
#8101=CYLINDRICAL_SURFACE('',#9263,3.5);
#8102=CYLINDRICAL_SURFACE('',#9272,3.5);
#8103=CYLINDRICAL_SURFACE('',#9274,3.5);
#8104=CYLINDRICAL_SURFACE('',#9276,5.);
#8105=CYLINDRICAL_SURFACE('',#9279,2.);
#8106=CYLINDRICAL_SURFACE('',#9286,2.);
#8107=CYLINDRICAL_SURFACE('',#9288,5.);
#8108=CYLINDRICAL_SURFACE('',#9295,1.5);
#8109=CYLINDRICAL_SURFACE('',#9302,2.);
#8110=CYLINDRICAL_SURFACE('',#9307,4.);
#8111=CYLINDRICAL_SURFACE('',#9310,2.);
#8112=CYLINDRICAL_SURFACE('',#9318,1.5);
#8113=CYLINDRICAL_SURFACE('',#9320,4.);
#8114=CYLINDRICAL_SURFACE('',#9330,3.5);
#8115=CYLINDRICAL_SURFACE('',#9332,3.5);
#8116=CYLINDRICAL_SURFACE('',#9337,2.);
#8117=CYLINDRICAL_SURFACE('',#9339,5.);
#8118=CYLINDRICAL_SURFACE('',#9346,3.5);
#8119=CYLINDRICAL_SURFACE('',#9349,5.);
#8120=CYLINDRICAL_SURFACE('',#9355,2.942);
#8121=CYLINDRICAL_SURFACE('',#9357,2.942);
#8122=CYLINDRICAL_SURFACE('',#9358,2.942);
#8123=CYLINDRICAL_SURFACE('',#9359,2.942);
#8124=CYLINDRICAL_SURFACE('',#9360,2.942);
#8125=CYLINDRICAL_SURFACE('',#9361,2.942);
#8126=CYLINDRICAL_SURFACE('',#9362,2.942);
#8127=CYLINDRICAL_SURFACE('',#9363,2.942);
#8128=CYLINDRICAL_SURFACE('',#9364,2.942);
#8129=CYLINDRICAL_SURFACE('',#9365,2.942);
#8130=CYLINDRICAL_SURFACE('',#9366,2.942);
#8131=CYLINDRICAL_SURFACE('',#9367,2.942);
#8132=CYLINDRICAL_SURFACE('',#9368,2.942);
#8133=CYLINDRICAL_SURFACE('',#9369,2.942);
#8134=CYLINDRICAL_SURFACE('',#9370,2.942);
#8135=CYLINDRICAL_SURFACE('',#9371,2.942);
#8136=CYLINDRICAL_SURFACE('',#9372,2.942);
#8137=CYLINDRICAL_SURFACE('',#9373,2.942);
#8138=CYLINDRICAL_SURFACE('',#9374,2.942);
#8139=CYLINDRICAL_SURFACE('',#9375,2.37175);
#8140=CYLINDRICAL_SURFACE('',#9377,2.37175);
#8141=CYLINDRICAL_SURFACE('',#9378,2.37175);
#8142=CYLINDRICAL_SURFACE('',#9379,2.37175);
#8143=CYLINDRICAL_SURFACE('',#9380,2.37175);
#8144=CYLINDRICAL_SURFACE('',#9381,2.37175);
#8145=CYLINDRICAL_SURFACE('',#9382,2.37175);
#8146=CYLINDRICAL_SURFACE('',#9383,2.37175);
#8147=CYLINDRICAL_SURFACE('',#9384,2.37175);
#8148=CYLINDRICAL_SURFACE('',#9385,2.37175);
#8149=CYLINDRICAL_SURFACE('',#9386,2.37175);
#8150=CYLINDRICAL_SURFACE('',#9387,2.37175);
#8151=CYLINDRICAL_SURFACE('',#9388,2.37175);
#8152=CYLINDRICAL_SURFACE('',#9389,2.37175);
#8153=CYLINDRICAL_SURFACE('',#9390,2.37175);
#8154=CYLINDRICAL_SURFACE('',#9391,2.37175);
#8155=CYLINDRICAL_SURFACE('',#9392,2.37175);
#8156=CYLINDRICAL_SURFACE('',#9393,2.37175);
#8157=CYLINDRICAL_SURFACE('',#9394,2.37175);
#8158=CYLINDRICAL_SURFACE('',#9398,2.37175);
#8159=CYLINDRICAL_SURFACE('',#9400,2.942);
#8160=CYLINDRICAL_SURFACE('',#9410,5.);
#8161=CYLINDRICAL_SURFACE('',#9415,2.942);
#8162=CYLINDRICAL_SURFACE('',#9417,2.942);
#8163=CYLINDRICAL_SURFACE('',#9418,2.942);
#8164=CYLINDRICAL_SURFACE('',#9419,2.942);
#8165=CYLINDRICAL_SURFACE('',#9420,2.942);
#8166=CYLINDRICAL_SURFACE('',#9421,2.942);
#8167=CYLINDRICAL_SURFACE('',#9422,2.942);
#8168=CYLINDRICAL_SURFACE('',#9423,2.942);
#8169=CYLINDRICAL_SURFACE('',#9424,2.942);
#8170=CYLINDRICAL_SURFACE('',#9425,2.942);
#8171=CYLINDRICAL_SURFACE('',#9426,2.942);
#8172=CYLINDRICAL_SURFACE('',#9427,2.37175);
#8173=CYLINDRICAL_SURFACE('',#9429,2.37175);
#8174=CYLINDRICAL_SURFACE('',#9430,2.37175);
#8175=CYLINDRICAL_SURFACE('',#9431,2.37175);
#8176=CYLINDRICAL_SURFACE('',#9432,2.37175);
#8177=CYLINDRICAL_SURFACE('',#9433,2.37175);
#8178=CYLINDRICAL_SURFACE('',#9434,2.37175);
#8179=CYLINDRICAL_SURFACE('',#9435,2.37175);
#8180=CYLINDRICAL_SURFACE('',#9436,2.37175);
#8181=CYLINDRICAL_SURFACE('',#9437,2.37175);
#8182=CYLINDRICAL_SURFACE('',#9438,2.37175);
#8183=CYLINDRICAL_SURFACE('',#9442,2.37175);
#8184=CYLINDRICAL_SURFACE('',#9444,2.942);
#8185=CYLINDRICAL_SURFACE('',#9454,5.);
#8186=CYLINDRICAL_SURFACE('',#9459,3.5);
#8187=CYLINDRICAL_SURFACE('',#9462,7.);
#8188=CYLINDRICAL_SURFACE('',#9468,2.5175);
#8189=CYLINDRICAL_SURFACE('',#9470,2.5175);
#8190=CYLINDRICAL_SURFACE('',#9471,2.5175);
#8191=CYLINDRICAL_SURFACE('',#9472,2.5175);
#8192=CYLINDRICAL_SURFACE('',#9473,2.5175);
#8193=CYLINDRICAL_SURFACE('',#9475,3.0735);
#8194=CYLINDRICAL_SURFACE('',#9477,3.0735);
#8195=CYLINDRICAL_SURFACE('',#9478,3.0735);
#8196=CYLINDRICAL_SURFACE('',#9479,3.0735);
#8197=CYLINDRICAL_SURFACE('',#9480,3.0735);
#8198=CYLINDRICAL_SURFACE('',#9482,3.0735);
#8199=CYLINDRICAL_SURFACE('',#9484,2.5175);
#8200=ADVANCED_FACE('',(#452),#7887,.F.);
#8201=ADVANCED_FACE('',(#453),#7888,.F.);
#8202=ADVANCED_FACE('',(#454),#7889,.F.);
#8203=ADVANCED_FACE('',(#455),#7890,.F.);
#8204=ADVANCED_FACE('',(#456),#7891,.F.);
#8205=ADVANCED_FACE('',(#457),#7892,.F.);
#8206=ADVANCED_FACE('',(#458),#7893,.F.);
#8207=ADVANCED_FACE('',(#459),#7894,.F.);
#8208=ADVANCED_FACE('',(#460),#7895,.F.);
#8209=ADVANCED_FACE('',(#461),#7896,.F.);
#8210=ADVANCED_FACE('',(#462),#7897,.F.);
#8211=ADVANCED_FACE('',(#463),#7898,.F.);
#8212=ADVANCED_FACE('',(#464),#7899,.F.);
#8213=ADVANCED_FACE('',(#465),#7900,.F.);
#8214=ADVANCED_FACE('',(#466),#7901,.F.);
#8215=ADVANCED_FACE('',(#467),#7902,.F.);
#8216=ADVANCED_FACE('',(#468),#7903,.F.);
#8217=ADVANCED_FACE('',(#469),#7904,.F.);
#8218=ADVANCED_FACE('',(#470),#7905,.F.);
#8219=ADVANCED_FACE('',(#471),#7906,.F.);
#8220=ADVANCED_FACE('',(#472),#7907,.F.);
#8221=ADVANCED_FACE('',(#473),#7908,.F.);
#8222=ADVANCED_FACE('',(#474),#7909,.F.);
#8223=ADVANCED_FACE('',(#475),#7910,.F.);
#8224=ADVANCED_FACE('',(#476),#7911,.F.);
#8225=ADVANCED_FACE('',(#477),#7912,.F.);
#8226=ADVANCED_FACE('',(#478),#7913,.F.);
#8227=ADVANCED_FACE('',(#479),#7914,.F.);
#8228=ADVANCED_FACE('',(#480),#7915,.F.);
#8229=ADVANCED_FACE('',(#481),#7916,.F.);
#8230=ADVANCED_FACE('',(#482),#7917,.F.);
#8231=ADVANCED_FACE('',(#483),#7918,.F.);
#8232=ADVANCED_FACE('',(#484),#7919,.F.);
#8233=ADVANCED_FACE('',(#485),#7920,.F.);
#8234=ADVANCED_FACE('',(#486),#7921,.F.);
#8235=ADVANCED_FACE('',(#487),#7922,.F.);
#8236=ADVANCED_FACE('',(#488),#7923,.F.);
#8237=ADVANCED_FACE('',(#489),#7924,.F.);
#8238=ADVANCED_FACE('',(#490),#7925,.F.);
#8239=ADVANCED_FACE('',(#491),#7926,.F.);
#8240=ADVANCED_FACE('',(#492),#7927,.F.);
#8241=ADVANCED_FACE('',(#493),#7928,.F.);
#8242=ADVANCED_FACE('',(#494),#7929,.F.);
#8243=ADVANCED_FACE('',(#495),#7930,.F.);
#8244=ADVANCED_FACE('',(#496),#7931,.F.);
#8245=ADVANCED_FACE('',(#497),#7932,.F.);
#8246=ADVANCED_FACE('',(#498),#7933,.F.);
#8247=ADVANCED_FACE('',(#499),#7934,.F.);
#8248=ADVANCED_FACE('',(#500),#7935,.F.);
#8249=ADVANCED_FACE('',(#501),#7936,.F.);
#8250=ADVANCED_FACE('',(#502),#7937,.F.);
#8251=ADVANCED_FACE('',(#503),#7938,.F.);
#8252=ADVANCED_FACE('',(#504),#7939,.F.);
#8253=ADVANCED_FACE('',(#505),#7940,.F.);
#8254=ADVANCED_FACE('',(#506),#7941,.F.);
#8255=ADVANCED_FACE('',(#507),#7942,.F.);
#8256=ADVANCED_FACE('',(#508),#7943,.F.);
#8257=ADVANCED_FACE('',(#509),#7944,.F.);
#8258=ADVANCED_FACE('',(#510),#7945,.F.);
#8259=ADVANCED_FACE('',(#511),#7946,.F.);
#8260=ADVANCED_FACE('',(#512),#7947,.F.);
#8261=ADVANCED_FACE('',(#513),#7948,.F.);
#8262=ADVANCED_FACE('',(#514),#7949,.F.);
#8263=ADVANCED_FACE('',(#515),#7950,.F.);
#8264=ADVANCED_FACE('',(#516),#7951,.F.);
#8265=ADVANCED_FACE('',(#517),#7952,.F.);
#8266=ADVANCED_FACE('',(#518),#7953,.F.);
#8267=ADVANCED_FACE('',(#519),#7954,.F.);
#8268=ADVANCED_FACE('',(#520),#7955,.F.);
#8269=ADVANCED_FACE('',(#521),#7956,.F.);
#8270=ADVANCED_FACE('',(#522),#7957,.F.);
#8271=ADVANCED_FACE('',(#523),#7958,.F.);
#8272=ADVANCED_FACE('',(#524),#7959,.F.);
#8273=ADVANCED_FACE('',(#525),#7960,.F.);
#8274=ADVANCED_FACE('',(#526),#7961,.F.);
#8275=ADVANCED_FACE('',(#527),#7962,.F.);
#8276=ADVANCED_FACE('',(#528),#7963,.F.);
#8277=ADVANCED_FACE('',(#529),#7964,.F.);
#8278=ADVANCED_FACE('',(#530),#7965,.F.);
#8279=ADVANCED_FACE('',(#531),#7966,.F.);
#8280=ADVANCED_FACE('',(#532),#7967,.F.);
#8281=ADVANCED_FACE('',(#533),#7968,.F.);
#8282=ADVANCED_FACE('',(#534),#7969,.F.);
#8283=ADVANCED_FACE('',(#535),#7970,.F.);
#8284=ADVANCED_FACE('',(#536),#7971,.F.);
#8285=ADVANCED_FACE('',(#537),#7972,.F.);
#8286=ADVANCED_FACE('',(#538),#7973,.F.);
#8287=ADVANCED_FACE('',(#539),#7974,.F.);
#8288=ADVANCED_FACE('',(#540),#7975,.F.);
#8289=ADVANCED_FACE('',(#541),#7976,.F.);
#8290=ADVANCED_FACE('',(#542),#7977,.F.);
#8291=ADVANCED_FACE('',(#543),#7978,.F.);
#8292=ADVANCED_FACE('',(#544),#7979,.F.);
#8293=ADVANCED_FACE('',(#545),#7980,.F.);
#8294=ADVANCED_FACE('',(#546),#7981,.F.);
#8295=ADVANCED_FACE('',(#547),#7982,.F.);
#8296=ADVANCED_FACE('',(#548),#7983,.F.);
#8297=ADVANCED_FACE('',(#549),#7984,.F.);
#8298=ADVANCED_FACE('',(#550),#7985,.F.);
#8299=ADVANCED_FACE('',(#551),#7986,.F.);
#8300=ADVANCED_FACE('',(#552),#7987,.F.);
#8301=ADVANCED_FACE('',(#553),#7988,.F.);
#8302=ADVANCED_FACE('',(#554),#7989,.F.);
#8303=ADVANCED_FACE('',(#555),#7990,.F.);
#8304=ADVANCED_FACE('',(#556),#7991,.F.);
#8305=ADVANCED_FACE('',(#557),#7992,.F.);
#8306=ADVANCED_FACE('',(#558),#7993,.F.);
#8307=ADVANCED_FACE('',(#559),#7994,.F.);
#8308=ADVANCED_FACE('',(#560),#7995,.F.);
#8309=ADVANCED_FACE('',(#561),#7996,.F.);
#8310=ADVANCED_FACE('',(#562),#7997,.F.);
#8311=ADVANCED_FACE('',(#563),#7998,.F.);
#8312=ADVANCED_FACE('',(#564),#7999,.F.);
#8313=ADVANCED_FACE('',(#565),#8000,.F.);
#8314=ADVANCED_FACE('',(#566),#8001,.F.);
#8315=ADVANCED_FACE('',(#567),#8002,.F.);
#8316=ADVANCED_FACE('',(#568),#8003,.F.);
#8317=ADVANCED_FACE('',(#569),#8004,.F.);
#8318=ADVANCED_FACE('',(#570),#8005,.F.);
#8319=ADVANCED_FACE('',(#571),#8006,.F.);
#8320=ADVANCED_FACE('',(#572),#8007,.F.);
#8321=ADVANCED_FACE('',(#573),#8008,.F.);
#8322=ADVANCED_FACE('',(#574),#8009,.F.);
#8323=ADVANCED_FACE('',(#575),#8010,.F.);
#8324=ADVANCED_FACE('',(#576),#8011,.F.);
#8325=ADVANCED_FACE('',(#577),#8012,.F.);
#8326=ADVANCED_FACE('',(#578),#8013,.F.);
#8327=ADVANCED_FACE('',(#579),#8014,.F.);
#8328=ADVANCED_FACE('',(#580),#8015,.F.);
#8329=ADVANCED_FACE('',(#581),#8016,.F.);
#8330=ADVANCED_FACE('',(#582),#8017,.F.);
#8331=ADVANCED_FACE('',(#583),#8018,.F.);
#8332=ADVANCED_FACE('',(#584),#8019,.F.);
#8333=ADVANCED_FACE('',(#585),#8020,.F.);
#8334=ADVANCED_FACE('',(#586),#8021,.F.);
#8335=ADVANCED_FACE('',(#587),#8022,.F.);
#8336=ADVANCED_FACE('',(#588),#311,.F.);
#8337=ADVANCED_FACE('',(#589),#8023,.F.);
#8338=ADVANCED_FACE('',(#590),#293,.F.);
#8339=ADVANCED_FACE('',(#591),#294,.F.);
#8340=ADVANCED_FACE('',(#592),#8024,.F.);
#8341=ADVANCED_FACE('',(#593),#312,.F.);
#8342=ADVANCED_FACE('',(#594),#8025,.F.);
#8343=ADVANCED_FACE('',(#595),#295,.F.);
#8344=ADVANCED_FACE('',(#596),#296,.F.);
#8345=ADVANCED_FACE('',(#597),#8026,.F.);
#8346=ADVANCED_FACE('',(#598),#313,.F.);
#8347=ADVANCED_FACE('',(#599),#8027,.F.);
#8348=ADVANCED_FACE('',(#600),#297,.F.);
#8349=ADVANCED_FACE('',(#601),#298,.F.);
#8350=ADVANCED_FACE('',(#602),#8028,.F.);
#8351=ADVANCED_FACE('',(#603),#314,.F.);
#8352=ADVANCED_FACE('',(#604),#8029,.F.);
#8353=ADVANCED_FACE('',(#605),#299,.F.);
#8354=ADVANCED_FACE('',(#606),#300,.F.);
#8355=ADVANCED_FACE('',(#607),#8030,.F.);
#8356=ADVANCED_FACE('',(#608),#315,.F.);
#8357=ADVANCED_FACE('',(#609),#316,.F.);
#8358=ADVANCED_FACE('',(#610),#317,.F.);
#8359=ADVANCED_FACE('',(#611),#318,.F.);
#8360=ADVANCED_FACE('',(#612),#319,.T.);
#8361=ADVANCED_FACE('',(#613),#320,.T.);
#8362=ADVANCED_FACE('',(#614),#321,.T.);
#8363=ADVANCED_FACE('',(#615),#322,.T.);
#8364=ADVANCED_FACE('',(#616),#323,.T.);
#8365=ADVANCED_FACE('',(#617),#324,.T.);
#8366=ADVANCED_FACE('',(#618),#325,.T.);
#8367=ADVANCED_FACE('',(#619),#326,.T.);
#8368=ADVANCED_FACE('',(#620,#234),#327,.T.);
#8369=ADVANCED_FACE('',(#621,#235,#236,#237,#238,#239),#328,.F.);
#8370=ADVANCED_FACE('',(#622),#8031,.F.);
#8371=ADVANCED_FACE('',(#623),#8032,.F.);
#8372=ADVANCED_FACE('',(#624),#8033,.F.);
#8373=ADVANCED_FACE('',(#625),#8034,.F.);
#8374=ADVANCED_FACE('',(#626),#8035,.F.);
#8375=ADVANCED_FACE('',(#627),#329,.T.);
#8376=ADVANCED_FACE('',(#628),#330,.T.);
#8377=ADVANCED_FACE('',(#629),#331,.T.);
#8378=ADVANCED_FACE('',(#630),#332,.T.);
#8379=ADVANCED_FACE('',(#631,#240,#241,#242,#243,#244),#333,.T.);
#8380=ADVANCED_FACE('',(#632,#245,#246,#247,#248,#249),#334,.F.);
#8381=ADVANCED_FACE('',(#633),#335,.T.);
#8382=ADVANCED_FACE('',(#634),#336,.T.);
#8383=ADVANCED_FACE('',(#635),#337,.T.);
#8384=ADVANCED_FACE('',(#636),#338,.T.);
#8385=ADVANCED_FACE('',(#637),#339,.T.);
#8386=ADVANCED_FACE('',(#638),#340,.T.);
#8387=ADVANCED_FACE('',(#639),#341,.T.);
#8388=ADVANCED_FACE('',(#640),#342,.T.);
#8389=ADVANCED_FACE('',(#641,#250),#343,.T.);
#8390=ADVANCED_FACE('',(#642,#251),#344,.F.);
#8391=ADVANCED_FACE('',(#643),#8036,.F.);
#8392=ADVANCED_FACE('',(#644),#8037,.F.);
#8393=ADVANCED_FACE('',(#645),#8038,.F.);
#8394=ADVANCED_FACE('',(#646),#8039,.F.);
#8395=ADVANCED_FACE('',(#647),#8040,.F.);
#8396=ADVANCED_FACE('',(#648),#8041,.F.);
#8397=ADVANCED_FACE('',(#649),#8042,.F.);
#8398=ADVANCED_FACE('',(#650),#8043,.F.);
#8399=ADVANCED_FACE('',(#651),#8044,.F.);
#8400=ADVANCED_FACE('',(#652),#8045,.F.);
#8401=ADVANCED_FACE('',(#653),#8046,.F.);
#8402=ADVANCED_FACE('',(#654),#8047,.F.);
#8403=ADVANCED_FACE('',(#655),#8048,.F.);
#8404=ADVANCED_FACE('',(#656),#8049,.F.);
#8405=ADVANCED_FACE('',(#657),#8050,.F.);
#8406=ADVANCED_FACE('',(#658),#8051,.F.);
#8407=ADVANCED_FACE('',(#659),#8052,.F.);
#8408=ADVANCED_FACE('',(#660),#8053,.F.);
#8409=ADVANCED_FACE('',(#661),#8054,.F.);
#8410=ADVANCED_FACE('',(#662),#8055,.F.);
#8411=ADVANCED_FACE('',(#663),#8056,.F.);
#8412=ADVANCED_FACE('',(#664),#8057,.F.);
#8413=ADVANCED_FACE('',(#665),#8058,.F.);
#8414=ADVANCED_FACE('',(#666),#8059,.F.);
#8415=ADVANCED_FACE('',(#667),#8060,.F.);
#8416=ADVANCED_FACE('',(#668),#8061,.F.);
#8417=ADVANCED_FACE('',(#669),#8062,.F.);
#8418=ADVANCED_FACE('',(#670),#8063,.F.);
#8419=ADVANCED_FACE('',(#671),#8064,.F.);
#8420=ADVANCED_FACE('',(#672),#8065,.F.);
#8421=ADVANCED_FACE('',(#673),#8066,.F.);
#8422=ADVANCED_FACE('',(#674),#345,.T.);
#8423=ADVANCED_FACE('',(#675),#8067,.F.);
#8424=ADVANCED_FACE('',(#676),#301,.F.);
#8425=ADVANCED_FACE('',(#677),#302,.F.);
#8426=ADVANCED_FACE('',(#678),#8068,.F.);
#8427=ADVANCED_FACE('',(#679),#346,.F.);
#8428=ADVANCED_FACE('',(#680),#347,.F.);
#8429=ADVANCED_FACE('',(#681),#348,.F.);
#8430=ADVANCED_FACE('',(#682),#349,.F.);
#8431=ADVANCED_FACE('',(#683),#350,.F.);
#8432=ADVANCED_FACE('',(#684),#351,.F.);
#8433=ADVANCED_FACE('',(#685),#8069,.T.);
#8434=ADVANCED_FACE('',(#686,#252),#352,.F.);
#8435=ADVANCED_FACE('',(#687,#253),#353,.F.);
#8436=ADVANCED_FACE('',(#688),#8070,.T.);
#8437=ADVANCED_FACE('',(#689),#354,.T.);
#8438=ADVANCED_FACE('',(#690),#355,.T.);
#8439=ADVANCED_FACE('',(#691),#356,.T.);
#8440=ADVANCED_FACE('',(#692),#357,.T.);
#8441=ADVANCED_FACE('',(#693),#358,.T.);
#8442=ADVANCED_FACE('',(#694),#359,.T.);
#8443=ADVANCED_FACE('',(#695,#254),#360,.T.);
#8444=ADVANCED_FACE('',(#696,#255),#361,.T.);
#8445=ADVANCED_FACE('',(#697),#8071,.T.);
#8446=ADVANCED_FACE('',(#698,#256),#362,.F.);
#8447=ADVANCED_FACE('',(#699),#8072,.T.);
#8448=ADVANCED_FACE('',(#700,#257),#363,.T.);
#8449=ADVANCED_FACE('',(#701),#364,.F.);
#8450=ADVANCED_FACE('',(#702),#365,.F.);
#8451=ADVANCED_FACE('',(#703),#366,.F.);
#8452=ADVANCED_FACE('',(#704),#367,.F.);
#8453=ADVANCED_FACE('',(#705),#368,.F.);
#8454=ADVANCED_FACE('',(#706),#369,.F.);
#8455=ADVANCED_FACE('',(#707),#370,.T.);
#8456=ADVANCED_FACE('',(#708),#371,.T.);
#8457=ADVANCED_FACE('',(#709),#372,.T.);
#8458=ADVANCED_FACE('',(#710),#373,.T.);
#8459=ADVANCED_FACE('',(#711,#258),#374,.T.);
#8460=ADVANCED_FACE('',(#712,#259),#375,.F.);
#8461=ADVANCED_FACE('',(#713),#8073,.F.);
#8462=ADVANCED_FACE('',(#714),#8074,.T.);
#8463=ADVANCED_FACE('',(#715,#260),#376,.T.);
#8464=ADVANCED_FACE('',(#716,#261),#377,.F.);
#8465=ADVANCED_FACE('',(#717),#378,.F.);
#8466=ADVANCED_FACE('',(#718),#379,.F.);
#8467=ADVANCED_FACE('',(#719),#380,.F.);
#8468=ADVANCED_FACE('',(#720),#8075,.F.);
#8469=ADVANCED_FACE('',(#721),#8076,.T.);
#8470=ADVANCED_FACE('',(#722),#381,.T.);
#8471=ADVANCED_FACE('',(#723),#8077,.F.);
#8472=ADVANCED_FACE('',(#724),#8078,.T.);
#8473=ADVANCED_FACE('',(#725,#262),#382,.T.);
#8474=ADVANCED_FACE('',(#726,#263),#383,.F.);
#8475=ADVANCED_FACE('',(#727),#8079,.T.);
#8476=ADVANCED_FACE('',(#728),#8080,.T.);
#8477=ADVANCED_FACE('',(#729),#8081,.T.);
#8478=ADVANCED_FACE('',(#730),#8082,.T.);
#8479=ADVANCED_FACE('',(#731),#8083,.T.);
#8480=ADVANCED_FACE('',(#732),#8084,.T.);
#8481=ADVANCED_FACE('',(#733),#8085,.T.);
#8482=ADVANCED_FACE('',(#734),#8086,.T.);
#8483=ADVANCED_FACE('',(#735),#8087,.T.);
#8484=ADVANCED_FACE('',(#736),#8088,.T.);
#8485=ADVANCED_FACE('',(#737),#8089,.T.);
#8486=ADVANCED_FACE('',(#738),#8090,.T.);
#8487=ADVANCED_FACE('',(#739),#8091,.T.);
#8488=ADVANCED_FACE('',(#740),#8092,.T.);
#8489=ADVANCED_FACE('',(#741),#8093,.T.);
#8490=ADVANCED_FACE('',(#742),#8094,.T.);
#8491=ADVANCED_FACE('',(#743),#8095,.T.);
#8492=ADVANCED_FACE('',(#744),#8096,.T.);
#8493=ADVANCED_FACE('',(#745),#8097,.T.);
#8494=ADVANCED_FACE('',(#746),#8098,.T.);
#8495=ADVANCED_FACE('',(#747),#159,.T.);
#8496=ADVANCED_FACE('',(#748),#303,.F.);
#8497=ADVANCED_FACE('',(#749),#8099,.T.);
#8498=ADVANCED_FACE('',(#750),#304,.F.);
#8499=ADVANCED_FACE('',(#751),#8100,.T.);
#8500=ADVANCED_FACE('',(#752),#384,.F.);
#8501=ADVANCED_FACE('',(#753),#385,.F.);
#8502=ADVANCED_FACE('',(#754),#386,.F.);
#8503=ADVANCED_FACE('',(#755),#387,.F.);
#8504=ADVANCED_FACE('',(#756),#388,.F.);
#8505=ADVANCED_FACE('',(#757),#389,.F.);
#8506=ADVANCED_FACE('',(#758),#390,.F.);
#8507=ADVANCED_FACE('',(#759,#264),#391,.T.);
#8508=ADVANCED_FACE('',(#760),#8101,.T.);
#8509=ADVANCED_FACE('',(#761,#265),#392,.F.);
#8510=ADVANCED_FACE('',(#762),#393,.T.);
#8511=ADVANCED_FACE('',(#763),#394,.F.);
#8512=ADVANCED_FACE('',(#764,#266,#267),#395,.T.);
#8513=ADVANCED_FACE('',(#765),#8102,.F.);
#8514=ADVANCED_FACE('',(#766),#8103,.F.);
#8515=ADVANCED_FACE('',(#767),#8104,.T.);
#8516=ADVANCED_FACE('',(#768),#8105,.F.);
#8517=ADVANCED_FACE('',(#769,#268),#396,.F.);
#8518=ADVANCED_FACE('',(#770,#269),#397,.T.);
#8519=ADVANCED_FACE('',(#771),#8106,.F.);
#8520=ADVANCED_FACE('',(#772),#8107,.T.);
#8521=ADVANCED_FACE('',(#773,#270),#398,.T.);
#8522=ADVANCED_FACE('',(#774,#271),#399,.T.);
#8523=ADVANCED_FACE('',(#775),#400,.T.);
#8524=ADVANCED_FACE('',(#776,#272,#273),#401,.F.);
#8525=ADVANCED_FACE('',(#777),#8108,.T.);
#8526=ADVANCED_FACE('',(#778,#274),#402,.F.);
#8527=ADVANCED_FACE('',(#779,#275),#403,.F.);
#8528=ADVANCED_FACE('',(#780),#8109,.T.);
#8529=ADVANCED_FACE('',(#781,#276),#404,.T.);
#8530=ADVANCED_FACE('',(#782),#8110,.T.);
#8531=ADVANCED_FACE('',(#783),#405,.F.);
#8532=ADVANCED_FACE('',(#784),#8111,.T.);
#8533=ADVANCED_FACE('',(#785),#406,.T.);
#8534=ADVANCED_FACE('',(#786),#407,.F.);
#8535=ADVANCED_FACE('',(#787),#408,.F.);
#8536=ADVANCED_FACE('',(#788),#409,.F.);
#8537=ADVANCED_FACE('',(#789),#8112,.F.);
#8538=ADVANCED_FACE('',(#790),#8113,.T.);
#8539=ADVANCED_FACE('',(#791),#410,.T.);
#8540=ADVANCED_FACE('',(#792),#411,.F.);
#8541=ADVANCED_FACE('',(#793),#412,.F.);
#8542=ADVANCED_FACE('',(#794,#277,#278),#413,.F.);
#8543=ADVANCED_FACE('',(#795),#414,.T.);
#8544=ADVANCED_FACE('',(#796),#8114,.F.);
#8545=ADVANCED_FACE('',(#797),#8115,.F.);
#8546=ADVANCED_FACE('',(#798,#279),#415,.T.);
#8547=ADVANCED_FACE('',(#799),#8116,.F.);
#8548=ADVANCED_FACE('',(#800),#8117,.T.);
#8549=ADVANCED_FACE('',(#801,#280),#416,.F.);
#8550=ADVANCED_FACE('',(#802),#417,.T.);
#8551=ADVANCED_FACE('',(#803),#418,.T.);
#8552=ADVANCED_FACE('',(#804,#281,#282),#419,.T.);
#8553=ADVANCED_FACE('',(#805),#8118,.F.);
#8554=ADVANCED_FACE('',(#806),#8119,.T.);
#8555=ADVANCED_FACE('',(#807,#283),#420,.T.);
#8556=ADVANCED_FACE('',(#808,#284),#421,.F.);
#8557=ADVANCED_FACE('',(#809),#8120,.T.);
#8558=ADVANCED_FACE('',(#810),#8121,.T.);
#8559=ADVANCED_FACE('',(#811),#8122,.T.);
#8560=ADVANCED_FACE('',(#812),#8123,.T.);
#8561=ADVANCED_FACE('',(#813),#8124,.T.);
#8562=ADVANCED_FACE('',(#814),#8125,.T.);
#8563=ADVANCED_FACE('',(#815),#8126,.T.);
#8564=ADVANCED_FACE('',(#816),#8127,.T.);
#8565=ADVANCED_FACE('',(#817),#8128,.T.);
#8566=ADVANCED_FACE('',(#818),#8129,.T.);
#8567=ADVANCED_FACE('',(#819),#8130,.T.);
#8568=ADVANCED_FACE('',(#820),#8131,.T.);
#8569=ADVANCED_FACE('',(#821),#8132,.T.);
#8570=ADVANCED_FACE('',(#822),#8133,.T.);
#8571=ADVANCED_FACE('',(#823),#8134,.T.);
#8572=ADVANCED_FACE('',(#824),#8135,.T.);
#8573=ADVANCED_FACE('',(#825),#8136,.T.);
#8574=ADVANCED_FACE('',(#826),#8137,.T.);
#8575=ADVANCED_FACE('',(#827),#8138,.T.);
#8576=ADVANCED_FACE('',(#828),#8139,.T.);
#8577=ADVANCED_FACE('',(#829),#8140,.T.);
#8578=ADVANCED_FACE('',(#830),#8141,.T.);
#8579=ADVANCED_FACE('',(#831),#8142,.T.);
#8580=ADVANCED_FACE('',(#832),#8143,.T.);
#8581=ADVANCED_FACE('',(#833),#8144,.T.);
#8582=ADVANCED_FACE('',(#834),#8145,.T.);
#8583=ADVANCED_FACE('',(#835),#8146,.T.);
#8584=ADVANCED_FACE('',(#836),#8147,.T.);
#8585=ADVANCED_FACE('',(#837),#8148,.T.);
#8586=ADVANCED_FACE('',(#838),#8149,.T.);
#8587=ADVANCED_FACE('',(#839),#8150,.T.);
#8588=ADVANCED_FACE('',(#840),#8151,.T.);
#8589=ADVANCED_FACE('',(#841),#8152,.T.);
#8590=ADVANCED_FACE('',(#842),#8153,.T.);
#8591=ADVANCED_FACE('',(#843),#8154,.T.);
#8592=ADVANCED_FACE('',(#844),#8155,.T.);
#8593=ADVANCED_FACE('',(#845),#8156,.T.);
#8594=ADVANCED_FACE('',(#846),#8157,.T.);
#8595=ADVANCED_FACE('',(#847),#160,.T.);
#8596=ADVANCED_FACE('',(#848),#305,.F.);
#8597=ADVANCED_FACE('',(#849),#8158,.T.);
#8598=ADVANCED_FACE('',(#850),#306,.F.);
#8599=ADVANCED_FACE('',(#851),#8159,.T.);
#8600=ADVANCED_FACE('',(#852),#422,.F.);
#8601=ADVANCED_FACE('',(#853),#423,.F.);
#8602=ADVANCED_FACE('',(#854),#424,.F.);
#8603=ADVANCED_FACE('',(#855),#425,.F.);
#8604=ADVANCED_FACE('',(#856),#426,.F.);
#8605=ADVANCED_FACE('',(#857),#427,.F.);
#8606=ADVANCED_FACE('',(#858),#428,.F.);
#8607=ADVANCED_FACE('',(#859,#285),#429,.T.);
#8608=ADVANCED_FACE('',(#860),#8160,.T.);
#8609=ADVANCED_FACE('',(#861,#286),#430,.F.);
#8610=ADVANCED_FACE('',(#862),#431,.T.);
#8611=ADVANCED_FACE('',(#863),#8161,.T.);
#8612=ADVANCED_FACE('',(#864),#8162,.T.);
#8613=ADVANCED_FACE('',(#865),#8163,.T.);
#8614=ADVANCED_FACE('',(#866),#8164,.T.);
#8615=ADVANCED_FACE('',(#867),#8165,.T.);
#8616=ADVANCED_FACE('',(#868),#8166,.T.);
#8617=ADVANCED_FACE('',(#869),#8167,.T.);
#8618=ADVANCED_FACE('',(#870),#8168,.T.);
#8619=ADVANCED_FACE('',(#871),#8169,.T.);
#8620=ADVANCED_FACE('',(#872),#8170,.T.);
#8621=ADVANCED_FACE('',(#873),#8171,.T.);
#8622=ADVANCED_FACE('',(#874),#8172,.T.);
#8623=ADVANCED_FACE('',(#875),#8173,.T.);
#8624=ADVANCED_FACE('',(#876),#8174,.T.);
#8625=ADVANCED_FACE('',(#877),#8175,.T.);
#8626=ADVANCED_FACE('',(#878),#8176,.T.);
#8627=ADVANCED_FACE('',(#879),#8177,.T.);
#8628=ADVANCED_FACE('',(#880),#8178,.T.);
#8629=ADVANCED_FACE('',(#881),#8179,.T.);
#8630=ADVANCED_FACE('',(#882),#8180,.T.);
#8631=ADVANCED_FACE('',(#883),#8181,.T.);
#8632=ADVANCED_FACE('',(#884),#8182,.T.);
#8633=ADVANCED_FACE('',(#885),#161,.T.);
#8634=ADVANCED_FACE('',(#886),#307,.F.);
#8635=ADVANCED_FACE('',(#887),#8183,.T.);
#8636=ADVANCED_FACE('',(#888),#308,.F.);
#8637=ADVANCED_FACE('',(#889),#8184,.T.);
#8638=ADVANCED_FACE('',(#890),#432,.F.);
#8639=ADVANCED_FACE('',(#891),#433,.F.);
#8640=ADVANCED_FACE('',(#892),#434,.F.);
#8641=ADVANCED_FACE('',(#893),#435,.F.);
#8642=ADVANCED_FACE('',(#894),#436,.F.);
#8643=ADVANCED_FACE('',(#895),#437,.F.);
#8644=ADVANCED_FACE('',(#896),#438,.F.);
#8645=ADVANCED_FACE('',(#897,#287),#439,.T.);
#8646=ADVANCED_FACE('',(#898),#8185,.T.);
#8647=ADVANCED_FACE('',(#899,#288),#440,.F.);
#8648=ADVANCED_FACE('',(#900),#441,.T.);
#8649=ADVANCED_FACE('',(#901),#8186,.F.);
#8650=ADVANCED_FACE('',(#902),#8187,.T.);
#8651=ADVANCED_FACE('',(#903,#289),#442,.T.);
#8652=ADVANCED_FACE('',(#904,#290),#443,.F.);
#8653=ADVANCED_FACE('',(#905),#8188,.F.);
#8654=ADVANCED_FACE('',(#906),#8189,.F.);
#8655=ADVANCED_FACE('',(#907),#8190,.F.);
#8656=ADVANCED_FACE('',(#908),#8191,.F.);
#8657=ADVANCED_FACE('',(#909),#8192,.F.);
#8658=ADVANCED_FACE('',(#910),#8193,.F.);
#8659=ADVANCED_FACE('',(#911),#8194,.F.);
#8660=ADVANCED_FACE('',(#912),#8195,.F.);
#8661=ADVANCED_FACE('',(#913),#8196,.F.);
#8662=ADVANCED_FACE('',(#914),#8197,.F.);
#8663=ADVANCED_FACE('',(#915),#8198,.F.);
#8664=ADVANCED_FACE('',(#916),#309,.F.);
#8665=ADVANCED_FACE('',(#917),#310,.F.);
#8666=ADVANCED_FACE('',(#918,#291),#444,.T.);
#8667=ADVANCED_FACE('',(#919),#8199,.F.);
#8668=ADVANCED_FACE('',(#920),#445,.T.);
#8669=ADVANCED_FACE('',(#921),#446,.T.);
#8670=ADVANCED_FACE('',(#922),#447,.T.);
#8671=ADVANCED_FACE('',(#923),#448,.T.);
#8672=ADVANCED_FACE('',(#924),#449,.T.);
#8673=ADVANCED_FACE('',(#925),#450,.T.);
#8674=ADVANCED_FACE('',(#926,#292),#451,.F.);
#8675=CLOSED_SHELL('',(#8200,#8201,#8202,#8203,#8204,#8205,#8206,#8207,
#8208,#8209,#8210,#8211,#8212,#8213,#8214,#8215,#8216,#8217,#8218,#8219,
#8220,#8221,#8222,#8223,#8224,#8225,#8226,#8227,#8228,#8229,#8230,#8231,
#8232,#8233,#8234,#8235,#8236,#8237,#8238,#8239,#8240,#8241,#8242,#8243,
#8244,#8245,#8246,#8247,#8248,#8249,#8250,#8251,#8252,#8253,#8254,#8255,
#8256,#8257,#8258,#8259,#8260,#8261,#8262,#8263,#8264,#8265,#8266,#8267,
#8268,#8269,#8270,#8271,#8272,#8273,#8274,#8275,#8276,#8277,#8278,#8279,
#8280,#8281,#8282,#8283,#8284,#8285,#8286,#8287,#8288,#8289,#8290,#8291,
#8292,#8293,#8294,#8295,#8296,#8297,#8298,#8299,#8300,#8301,#8302,#8303,
#8304,#8305,#8306,#8307,#8308,#8309,#8310,#8311,#8312,#8313,#8314,#8315,
#8316,#8317,#8318,#8319,#8320,#8321,#8322,#8323,#8324,#8325,#8326,#8327,
#8328,#8329,#8330,#8331,#8332,#8333,#8334,#8335,#8336,#8337,#8338,#8339,
#8340,#8341,#8342,#8343,#8344,#8345,#8346,#8347,#8348,#8349,#8350,#8351,
#8352,#8353,#8354,#8355,#8356,#8357,#8358,#8359,#8360,#8361,#8362,#8363,
#8364,#8365,#8366,#8367,#8368,#8369));
#8676=CLOSED_SHELL('',(#8370,#8371,#8372,#8373,#8374,#8375,#8376,#8377,
#8378,#8379,#8380));
#8677=CLOSED_SHELL('',(#8381,#8382,#8383,#8384,#8385,#8386,#8387,#8388,
#8389,#8390));
#8678=CLOSED_SHELL('',(#8391,#8392,#8393,#8394,#8395,#8396,#8397,#8398,
#8399,#8400,#8401,#8402,#8403,#8404,#8405,#8406,#8407,#8408,#8409,#8410,
#8411,#8412,#8413,#8414,#8415,#8416,#8417,#8418,#8419,#8420,#8421,#8422,
#8423,#8424,#8425,#8426,#8427,#8428,#8429,#8430,#8431,#8432,#8433,#8434,
#8435,#8436,#8437,#8438,#8439,#8440,#8441,#8442,#8443,#8444,#8445,#8446,
#8447,#8448));
#8679=CLOSED_SHELL('',(#8449,#8450,#8451,#8452,#8453,#8454,#8455,#8456,
#8457,#8458,#8459,#8460));
#8680=CLOSED_SHELL('',(#8461,#8462,#8463,#8464));
#8681=CLOSED_SHELL('',(#8465,#8466,#8467,#8468,#8469,#8470));
#8682=CLOSED_SHELL('',(#8471,#8472,#8473,#8474));
#8683=CLOSED_SHELL('',(#8475,#8476,#8477,#8478,#8479,#8480,#8481,#8482,
#8483,#8484,#8485,#8486,#8487,#8488,#8489,#8490,#8491,#8492,#8493,#8494,
#8495,#8496,#8497,#8498,#8499,#8500,#8501,#8502,#8503,#8504,#8505,#8506,
#8507,#8508,#8509,#8510));
#8684=CLOSED_SHELL('',(#8511,#8512,#8513,#8514,#8515,#8516,#8517,#8518,
#8519,#8520,#8521,#8522,#8523,#8524));
#8685=CLOSED_SHELL('',(#8525,#8526,#8527,#8528,#8529,#8530,#8531,#8532,
#8533));
#8686=CLOSED_SHELL('',(#8534,#8535,#8536,#8537,#8538,#8539));
#8687=CLOSED_SHELL('',(#8540,#8541,#8542,#8543,#8544,#8545,#8546,#8547,
#8548,#8549,#8550,#8551,#8552));
#8688=CLOSED_SHELL('',(#8553,#8554,#8555,#8556));
#8689=CLOSED_SHELL('',(#8557,#8558,#8559,#8560,#8561,#8562,#8563,#8564,
#8565,#8566,#8567,#8568,#8569,#8570,#8571,#8572,#8573,#8574,#8575,#8576,
#8577,#8578,#8579,#8580,#8581,#8582,#8583,#8584,#8585,#8586,#8587,#8588,
#8589,#8590,#8591,#8592,#8593,#8594,#8595,#8596,#8597,#8598,#8599,#8600,
#8601,#8602,#8603,#8604,#8605,#8606,#8607,#8608,#8609,#8610));
#8690=CLOSED_SHELL('',(#8611,#8612,#8613,#8614,#8615,#8616,#8617,#8618,
#8619,#8620,#8621,#8622,#8623,#8624,#8625,#8626,#8627,#8628,#8629,#8630,
#8631,#8632,#8633,#8634,#8635,#8636,#8637,#8638,#8639,#8640,#8641,#8642,
#8643,#8644,#8645,#8646,#8647,#8648));
#8691=CLOSED_SHELL('',(#8649,#8650,#8651,#8652));
#8692=CLOSED_SHELL('',(#8653,#8654,#8655,#8656,#8657,#8658,#8659,#8660,
#8661,#8662,#8663,#8664,#8665,#8666,#8667,#8668,#8669,#8670,#8671,#8672,
#8673,#8674));
#8693=DERIVED_UNIT_ELEMENT(#8729,1.);
#8694=DERIVED_UNIT_ELEMENT(#32629,-3.);
#8695=DERIVED_UNIT_ELEMENT(#8729,1.);
#8696=DERIVED_UNIT_ELEMENT(#32629,-3.);
#8697=DERIVED_UNIT_ELEMENT(#8729,1.);
#8698=DERIVED_UNIT_ELEMENT(#32629,-3.);
#8699=DERIVED_UNIT_ELEMENT(#8729,1.);
#8700=DERIVED_UNIT_ELEMENT(#32629,-3.);
#8701=DERIVED_UNIT_ELEMENT(#8729,1.);
#8702=DERIVED_UNIT_ELEMENT(#32629,-3.);
#8703=DERIVED_UNIT_ELEMENT(#8729,1.);
#8704=DERIVED_UNIT_ELEMENT(#32629,-3.);
#8705=DERIVED_UNIT_ELEMENT(#8729,1.);
#8706=DERIVED_UNIT_ELEMENT(#32629,-3.);
#8707=DERIVED_UNIT_ELEMENT(#8729,1.);
#8708=DERIVED_UNIT_ELEMENT(#32629,-3.);
#8709=DERIVED_UNIT_ELEMENT(#8729,1.);
#8710=DERIVED_UNIT_ELEMENT(#32629,-3.);
#8711=DERIVED_UNIT_ELEMENT(#8729,1.);
#8712=DERIVED_UNIT_ELEMENT(#32629,-3.);
#8713=DERIVED_UNIT_ELEMENT(#8729,1.);
#8714=DERIVED_UNIT_ELEMENT(#32629,-3.);
#8715=DERIVED_UNIT_ELEMENT(#8729,1.);
#8716=DERIVED_UNIT_ELEMENT(#32629,-3.);
#8717=DERIVED_UNIT_ELEMENT(#8729,1.);
#8718=DERIVED_UNIT_ELEMENT(#32629,-3.);
#8719=DERIVED_UNIT_ELEMENT(#8729,1.);
#8720=DERIVED_UNIT_ELEMENT(#32629,-3.);
#8721=DERIVED_UNIT_ELEMENT(#8729,1.);
#8722=DERIVED_UNIT_ELEMENT(#32629,-3.);
#8723=DERIVED_UNIT_ELEMENT(#8729,1.);
#8724=DERIVED_UNIT_ELEMENT(#32629,-3.);
#8725=DERIVED_UNIT_ELEMENT(#8729,1.);
#8726=DERIVED_UNIT_ELEMENT(#32629,-3.);
#8727=DERIVED_UNIT_ELEMENT(#8729,1.);
#8728=DERIVED_UNIT_ELEMENT(#32629,-3.);
#8729=(
MASS_UNIT()
NAMED_UNIT(*)
SI_UNIT(.KILO.,.GRAM.)
);
#8730=DERIVED_UNIT((#8693,#8694));
#8731=DERIVED_UNIT((#8695,#8696));
#8732=DERIVED_UNIT((#8697,#8698));
#8733=DERIVED_UNIT((#8699,#8700));
#8734=DERIVED_UNIT((#8701,#8702));
#8735=DERIVED_UNIT((#8703,#8704));
#8736=DERIVED_UNIT((#8705,#8706));
#8737=DERIVED_UNIT((#8707,#8708));
#8738=DERIVED_UNIT((#8709,#8710));
#8739=DERIVED_UNIT((#8711,#8712));
#8740=DERIVED_UNIT((#8713,#8714));
#8741=DERIVED_UNIT((#8715,#8716));
#8742=DERIVED_UNIT((#8717,#8718));
#8743=DERIVED_UNIT((#8719,#8720));
#8744=DERIVED_UNIT((#8721,#8722));
#8745=DERIVED_UNIT((#8723,#8724));
#8746=DERIVED_UNIT((#8725,#8726));
#8747=DERIVED_UNIT((#8727,#8728));
#8748=MEASURE_REPRESENTATION_ITEM('density measure',
POSITIVE_RATIO_MEASURE(7850.),#8730);
#8749=MEASURE_REPRESENTATION_ITEM('density measure',
POSITIVE_RATIO_MEASURE(7850.),#8731);
#8750=MEASURE_REPRESENTATION_ITEM('density measure',
POSITIVE_RATIO_MEASURE(1250.),#8732);
#8751=MEASURE_REPRESENTATION_ITEM('density measure',
POSITIVE_RATIO_MEASURE(7850.),#8733);
#8752=MEASURE_REPRESENTATION_ITEM('density measure',
POSITIVE_RATIO_MEASURE(7850.),#8734);
#8753=MEASURE_REPRESENTATION_ITEM('density measure',
POSITIVE_RATIO_MEASURE(7850.),#8735);
#8754=MEASURE_REPRESENTATION_ITEM('density measure',
POSITIVE_RATIO_MEASURE(7850.),#8736);
#8755=MEASURE_REPRESENTATION_ITEM('density measure',
POSITIVE_RATIO_MEASURE(7850.),#8737);
#8756=MEASURE_REPRESENTATION_ITEM('density measure',
POSITIVE_RATIO_MEASURE(7850.),#8738);
#8757=MEASURE_REPRESENTATION_ITEM('density measure',
POSITIVE_RATIO_MEASURE(7850.),#8739);
#8758=MEASURE_REPRESENTATION_ITEM('density measure',
POSITIVE_RATIO_MEASURE(7850.),#8740);
#8759=MEASURE_REPRESENTATION_ITEM('density measure',
POSITIVE_RATIO_MEASURE(7850.),#8741);
#8760=MEASURE_REPRESENTATION_ITEM('density measure',
POSITIVE_RATIO_MEASURE(7850.),#8742);
#8761=MEASURE_REPRESENTATION_ITEM('density measure',
POSITIVE_RATIO_MEASURE(7850.),#8743);
#8762=MEASURE_REPRESENTATION_ITEM('density measure',
POSITIVE_RATIO_MEASURE(7850.),#8744);
#8763=MEASURE_REPRESENTATION_ITEM('density measure',
POSITIVE_RATIO_MEASURE(7850.),#8745);
#8764=MEASURE_REPRESENTATION_ITEM('density measure',
POSITIVE_RATIO_MEASURE(7850.),#8746);
#8765=MEASURE_REPRESENTATION_ITEM('density measure',
POSITIVE_RATIO_MEASURE(7850.),#8747);
#8766=PROPERTY_DEFINITION_REPRESENTATION(#8856,#8802);
#8767=PROPERTY_DEFINITION_REPRESENTATION(#8857,#8803);
#8768=PROPERTY_DEFINITION_REPRESENTATION(#8858,#8804);
#8769=PROPERTY_DEFINITION_REPRESENTATION(#8859,#8805);
#8770=PROPERTY_DEFINITION_REPRESENTATION(#8860,#8806);
#8771=PROPERTY_DEFINITION_REPRESENTATION(#8861,#8807);
#8772=PROPERTY_DEFINITION_REPRESENTATION(#8862,#8808);
#8773=PROPERTY_DEFINITION_REPRESENTATION(#8863,#8809);
#8774=PROPERTY_DEFINITION_REPRESENTATION(#8864,#8810);
#8775=PROPERTY_DEFINITION_REPRESENTATION(#8865,#8811);
#8776=PROPERTY_DEFINITION_REPRESENTATION(#8866,#8812);
#8777=PROPERTY_DEFINITION_REPRESENTATION(#8867,#8813);
#8778=PROPERTY_DEFINITION_REPRESENTATION(#8868,#8814);
#8779=PROPERTY_DEFINITION_REPRESENTATION(#8869,#8815);
#8780=PROPERTY_DEFINITION_REPRESENTATION(#8870,#8816);
#8781=PROPERTY_DEFINITION_REPRESENTATION(#8871,#8817);
#8782=PROPERTY_DEFINITION_REPRESENTATION(#8872,#8818);
#8783=PROPERTY_DEFINITION_REPRESENTATION(#8873,#8819);
#8784=PROPERTY_DEFINITION_REPRESENTATION(#8874,#8820);
#8785=PROPERTY_DEFINITION_REPRESENTATION(#8875,#8821);
#8786=PROPERTY_DEFINITION_REPRESENTATION(#8876,#8822);
#8787=PROPERTY_DEFINITION_REPRESENTATION(#8877,#8823);
#8788=PROPERTY_DEFINITION_REPRESENTATION(#8878,#8824);
#8789=PROPERTY_DEFINITION_REPRESENTATION(#8879,#8825);
#8790=PROPERTY_DEFINITION_REPRESENTATION(#8880,#8826);
#8791=PROPERTY_DEFINITION_REPRESENTATION(#8881,#8827);
#8792=PROPERTY_DEFINITION_REPRESENTATION(#8882,#8828);
#8793=PROPERTY_DEFINITION_REPRESENTATION(#8883,#8829);
#8794=PROPERTY_DEFINITION_REPRESENTATION(#8884,#8830);
#8795=PROPERTY_DEFINITION_REPRESENTATION(#8885,#8831);
#8796=PROPERTY_DEFINITION_REPRESENTATION(#8886,#8832);
#8797=PROPERTY_DEFINITION_REPRESENTATION(#8887,#8833);
#8798=PROPERTY_DEFINITION_REPRESENTATION(#8888,#8834);
#8799=PROPERTY_DEFINITION_REPRESENTATION(#8889,#8835);
#8800=PROPERTY_DEFINITION_REPRESENTATION(#8890,#8836);
#8801=PROPERTY_DEFINITION_REPRESENTATION(#8891,#8837);
#8802=REPRESENTATION('material name',(#8838),#32609);
#8803=REPRESENTATION('density',(#8748),#32609);
#8804=REPRESENTATION('material name',(#8839),#32610);
#8805=REPRESENTATION('density',(#8749),#32610);
#8806=REPRESENTATION('material name',(#8840),#32611);
#8807=REPRESENTATION('density',(#8750),#32611);
#8808=REPRESENTATION('material name',(#8841),#32612);
#8809=REPRESENTATION('density',(#8751),#32612);
#8810=REPRESENTATION('material name',(#8842),#32613);
#8811=REPRESENTATION('density',(#8752),#32613);
#8812=REPRESENTATION('material name',(#8843),#32614);
#8813=REPRESENTATION('density',(#8753),#32614);
#8814=REPRESENTATION('material name',(#8844),#32615);
#8815=REPRESENTATION('density',(#8754),#32615);
#8816=REPRESENTATION('material name',(#8845),#32616);
#8817=REPRESENTATION('density',(#8755),#32616);
#8818=REPRESENTATION('material name',(#8846),#32617);
#8819=REPRESENTATION('density',(#8756),#32617);
#8820=REPRESENTATION('material name',(#8847),#32618);
#8821=REPRESENTATION('density',(#8757),#32618);
#8822=REPRESENTATION('material name',(#8848),#32619);
#8823=REPRESENTATION('density',(#8758),#32619);
#8824=REPRESENTATION('material name',(#8849),#32620);
#8825=REPRESENTATION('density',(#8759),#32620);
#8826=REPRESENTATION('material name',(#8850),#32621);
#8827=REPRESENTATION('density',(#8760),#32621);
#8828=REPRESENTATION('material name',(#8851),#32622);
#8829=REPRESENTATION('density',(#8761),#32622);
#8830=REPRESENTATION('material name',(#8852),#32623);
#8831=REPRESENTATION('density',(#8762),#32623);
#8832=REPRESENTATION('material name',(#8853),#32624);
#8833=REPRESENTATION('density',(#8763),#32624);
#8834=REPRESENTATION('material name',(#8854),#32625);
#8835=REPRESENTATION('density',(#8764),#32625);
#8836=REPRESENTATION('material name',(#8855),#32626);
#8837=REPRESENTATION('density',(#8765),#32626);
#8838=DESCRIPTIVE_REPRESENTATION_ITEM('Steel','Steel');
#8839=DESCRIPTIVE_REPRESENTATION_ITEM('Steel','Steel');
#8840=DESCRIPTIVE_REPRESENTATION_ITEM('Rubber, Silicone',
'Rubber, Silicone');
#8841=DESCRIPTIVE_REPRESENTATION_ITEM('Steel','Steel');
#8842=DESCRIPTIVE_REPRESENTATION_ITEM('Steel','Steel');
#8843=DESCRIPTIVE_REPRESENTATION_ITEM('Steel','Steel');
#8844=DESCRIPTIVE_REPRESENTATION_ITEM('Steel','Steel');
#8845=DESCRIPTIVE_REPRESENTATION_ITEM('Steel','Steel');
#8846=DESCRIPTIVE_REPRESENTATION_ITEM('Steel','Steel');
#8847=DESCRIPTIVE_REPRESENTATION_ITEM('Steel','Steel');
#8848=DESCRIPTIVE_REPRESENTATION_ITEM('Steel','Steel');
#8849=DESCRIPTIVE_REPRESENTATION_ITEM('Steel','Steel');
#8850=DESCRIPTIVE_REPRESENTATION_ITEM('Steel','Steel');
#8851=DESCRIPTIVE_REPRESENTATION_ITEM('Steel','Steel');
#8852=DESCRIPTIVE_REPRESENTATION_ITEM('Steel','Steel');
#8853=DESCRIPTIVE_REPRESENTATION_ITEM('Steel','Steel');
#8854=DESCRIPTIVE_REPRESENTATION_ITEM('Steel','Steel');
#8855=DESCRIPTIVE_REPRESENTATION_ITEM('Steel','Steel');
#8856=PROPERTY_DEFINITION('material property','material name',#32728);
#8857=PROPERTY_DEFINITION('material property','density of part',#32728);
#8858=PROPERTY_DEFINITION('material property','material name',#32729);
#8859=PROPERTY_DEFINITION('material property','density of part',#32729);
#8860=PROPERTY_DEFINITION('material property','material name',#32730);
#8861=PROPERTY_DEFINITION('material property','density of part',#32730);
#8862=PROPERTY_DEFINITION('material property','material name',#32731);
#8863=PROPERTY_DEFINITION('material property','density of part',#32731);
#8864=PROPERTY_DEFINITION('material property','material name',#32732);
#8865=PROPERTY_DEFINITION('material property','density of part',#32732);
#8866=PROPERTY_DEFINITION('material property','material name',#32733);
#8867=PROPERTY_DEFINITION('material property','density of part',#32733);
#8868=PROPERTY_DEFINITION('material property','material name',#32734);
#8869=PROPERTY_DEFINITION('material property','density of part',#32734);
#8870=PROPERTY_DEFINITION('material property','material name',#32735);
#8871=PROPERTY_DEFINITION('material property','density of part',#32735);
#8872=PROPERTY_DEFINITION('material property','material name',#32736);
#8873=PROPERTY_DEFINITION('material property','density of part',#32736);
#8874=PROPERTY_DEFINITION('material property','material name',#32737);
#8875=PROPERTY_DEFINITION('material property','density of part',#32737);
#8876=PROPERTY_DEFINITION('material property','material name',#32738);
#8877=PROPERTY_DEFINITION('material property','density of part',#32738);
#8878=PROPERTY_DEFINITION('material property','material name',#32739);
#8879=PROPERTY_DEFINITION('material property','density of part',#32739);
#8880=PROPERTY_DEFINITION('material property','material name',#32740);
#8881=PROPERTY_DEFINITION('material property','density of part',#32740);
#8882=PROPERTY_DEFINITION('material property','material name',#32741);
#8883=PROPERTY_DEFINITION('material property','density of part',#32741);
#8884=PROPERTY_DEFINITION('material property','material name',#32742);
#8885=PROPERTY_DEFINITION('material property','density of part',#32742);
#8886=PROPERTY_DEFINITION('material property','material name',#32743);
#8887=PROPERTY_DEFINITION('material property','density of part',#32743);
#8888=PROPERTY_DEFINITION('material property','material name',#32744);
#8889=PROPERTY_DEFINITION('material property','density of part',#32744);
#8890=PROPERTY_DEFINITION('material property','material name',#32745);
#8891=PROPERTY_DEFINITION('material property','density of part',#32745);
#8892=AXIS2_PLACEMENT_3D('',#11349,#9529,#9530);
#8893=AXIS2_PLACEMENT_3D('',#11350,#9531,#9532);
#8894=AXIS2_PLACEMENT_3D('',#11351,#9533,#9534);
#8895=AXIS2_PLACEMENT_3D('',#11361,#9536,#9537);
#8896=AXIS2_PLACEMENT_3D('',#11364,#9539,#9540);
#8897=AXIS2_PLACEMENT_3D('',#11366,#9541,#9542);
#8898=AXIS2_PLACEMENT_3D('',#11377,#9543,#9544);
#8899=AXIS2_PLACEMENT_3D('',#11425,#9546,#9547);
#8900=AXIS2_PLACEMENT_3D('',#11476,#9549,#9550);
#8901=AXIS2_PLACEMENT_3D('',#11524,#9552,#9553);
#8902=AXIS2_PLACEMENT_3D('',#11572,#9555,#9556);
#8903=AXIS2_PLACEMENT_3D('',#11623,#9558,#9559);
#8904=AXIS2_PLACEMENT_3D('',#11674,#9561,#9562);
#8905=AXIS2_PLACEMENT_3D('',#11722,#9564,#9565);
#8906=AXIS2_PLACEMENT_3D('',#11773,#9567,#9568);
#8907=AXIS2_PLACEMENT_3D('',#11824,#9570,#9571);
#8908=AXIS2_PLACEMENT_3D('',#11872,#9573,#9574);
#8909=AXIS2_PLACEMENT_3D('',#11920,#9576,#9577);
#8910=AXIS2_PLACEMENT_3D('',#11971,#9579,#9580);
#8911=AXIS2_PLACEMENT_3D('',#12022,#9582,#9583);
#8912=AXIS2_PLACEMENT_3D('',#12070,#9585,#9586);
#8913=AXIS2_PLACEMENT_3D('',#12121,#9588,#9589);
#8914=AXIS2_PLACEMENT_3D('',#12140,#9591,#9592);
#8915=AXIS2_PLACEMENT_3D('',#12160,#9593,#9594);
#8916=AXIS2_PLACEMENT_3D('',#12174,#9596,#9597);
#8917=AXIS2_PLACEMENT_3D('',#12184,#9598,#9599);
#8918=AXIS2_PLACEMENT_3D('',#12208,#9601,#9602);
#8919=AXIS2_PLACEMENT_3D('',#12233,#9604,#9605);
#8920=AXIS2_PLACEMENT_3D('',#12257,#9607,#9608);
#8921=AXIS2_PLACEMENT_3D('',#12282,#9610,#9611);
#8922=AXIS2_PLACEMENT_3D('',#12306,#9613,#9614);
#8923=AXIS2_PLACEMENT_3D('',#12331,#9616,#9617);
#8924=AXIS2_PLACEMENT_3D('',#12356,#9619,#9620);
#8925=AXIS2_PLACEMENT_3D('',#12380,#9622,#9623);
#8926=AXIS2_PLACEMENT_3D('',#12405,#9625,#9626);
#8927=AXIS2_PLACEMENT_3D('',#12429,#9628,#9629);
#8928=AXIS2_PLACEMENT_3D('',#12454,#9631,#9632);
#8929=AXIS2_PLACEMENT_3D('',#12478,#9634,#9635);
#8930=AXIS2_PLACEMENT_3D('',#12503,#9637,#9638);
#8931=AXIS2_PLACEMENT_3D('',#12528,#9640,#9641);
#8932=AXIS2_PLACEMENT_3D('',#12552,#9643,#9644);
#8933=AXIS2_PLACEMENT_3D('',#12563,#9646,#9647);
#8934=AXIS2_PLACEMENT_3D('',#12569,#9648,#9649);
#8935=AXIS2_PLACEMENT_3D('',#12579,#9651,#9652);
#8936=AXIS2_PLACEMENT_3D('',#12582,#9654,#9655);
#8937=AXIS2_PLACEMENT_3D('',#12584,#9656,#9657);
#8938=AXIS2_PLACEMENT_3D('',#12595,#9658,#9659);
#8939=AXIS2_PLACEMENT_3D('',#12643,#9661,#9662);
#8940=AXIS2_PLACEMENT_3D('',#12694,#9664,#9665);
#8941=AXIS2_PLACEMENT_3D('',#12742,#9667,#9668);
#8942=AXIS2_PLACEMENT_3D('',#12790,#9670,#9671);
#8943=AXIS2_PLACEMENT_3D('',#12841,#9673,#9674);
#8944=AXIS2_PLACEMENT_3D('',#12892,#9676,#9677);
#8945=AXIS2_PLACEMENT_3D('',#12940,#9679,#9680);
#8946=AXIS2_PLACEMENT_3D('',#12991,#9682,#9683);
#8947=AXIS2_PLACEMENT_3D('',#13042,#9685,#9686);
#8948=AXIS2_PLACEMENT_3D('',#13090,#9688,#9689);
#8949=AXIS2_PLACEMENT_3D('',#13138,#9691,#9692);
#8950=AXIS2_PLACEMENT_3D('',#13189,#9694,#9695);
#8951=AXIS2_PLACEMENT_3D('',#13240,#9697,#9698);
#8952=AXIS2_PLACEMENT_3D('',#13288,#9700,#9701);
#8953=AXIS2_PLACEMENT_3D('',#13339,#9703,#9704);
#8954=AXIS2_PLACEMENT_3D('',#13358,#9706,#9707);
#8955=AXIS2_PLACEMENT_3D('',#13378,#9708,#9709);
#8956=AXIS2_PLACEMENT_3D('',#13392,#9711,#9712);
#8957=AXIS2_PLACEMENT_3D('',#13402,#9713,#9714);
#8958=AXIS2_PLACEMENT_3D('',#13426,#9716,#9717);
#8959=AXIS2_PLACEMENT_3D('',#13451,#9719,#9720);
#8960=AXIS2_PLACEMENT_3D('',#13475,#9722,#9723);
#8961=AXIS2_PLACEMENT_3D('',#13500,#9725,#9726);
#8962=AXIS2_PLACEMENT_3D('',#13524,#9728,#9729);
#8963=AXIS2_PLACEMENT_3D('',#13549,#9731,#9732);
#8964=AXIS2_PLACEMENT_3D('',#13574,#9734,#9735);
#8965=AXIS2_PLACEMENT_3D('',#13598,#9737,#9738);
#8966=AXIS2_PLACEMENT_3D('',#13623,#9740,#9741);
#8967=AXIS2_PLACEMENT_3D('',#13647,#9743,#9744);
#8968=AXIS2_PLACEMENT_3D('',#13672,#9746,#9747);
#8969=AXIS2_PLACEMENT_3D('',#13696,#9749,#9750);
#8970=AXIS2_PLACEMENT_3D('',#13721,#9752,#9753);
#8971=AXIS2_PLACEMENT_3D('',#13746,#9755,#9756);
#8972=AXIS2_PLACEMENT_3D('',#13770,#9758,#9759);
#8973=AXIS2_PLACEMENT_3D('',#13781,#9761,#9762);
#8974=AXIS2_PLACEMENT_3D('',#13787,#9763,#9764);
#8975=AXIS2_PLACEMENT_3D('',#13797,#9766,#9767);
#8976=AXIS2_PLACEMENT_3D('',#13800,#9769,#9770);
#8977=AXIS2_PLACEMENT_3D('',#13802,#9771,#9772);
#8978=AXIS2_PLACEMENT_3D('',#13813,#9773,#9774);
#8979=AXIS2_PLACEMENT_3D('',#13861,#9776,#9777);
#8980=AXIS2_PLACEMENT_3D('',#13912,#9779,#9780);
#8981=AXIS2_PLACEMENT_3D('',#13960,#9782,#9783);
#8982=AXIS2_PLACEMENT_3D('',#14008,#9785,#9786);
#8983=AXIS2_PLACEMENT_3D('',#14059,#9788,#9789);
#8984=AXIS2_PLACEMENT_3D('',#14110,#9791,#9792);
#8985=AXIS2_PLACEMENT_3D('',#14158,#9794,#9795);
#8986=AXIS2_PLACEMENT_3D('',#14209,#9797,#9798);
#8987=AXIS2_PLACEMENT_3D('',#14260,#9800,#9801);
#8988=AXIS2_PLACEMENT_3D('',#14308,#9803,#9804);
#8989=AXIS2_PLACEMENT_3D('',#14356,#9806,#9807);
#8990=AXIS2_PLACEMENT_3D('',#14407,#9809,#9810);
#8991=AXIS2_PLACEMENT_3D('',#14458,#9812,#9813);
#8992=AXIS2_PLACEMENT_3D('',#14506,#9815,#9816);
#8993=AXIS2_PLACEMENT_3D('',#14557,#9818,#9819);
#8994=AXIS2_PLACEMENT_3D('',#14576,#9821,#9822);
#8995=AXIS2_PLACEMENT_3D('',#14596,#9823,#9824);
#8996=AXIS2_PLACEMENT_3D('',#14610,#9826,#9827);
#8997=AXIS2_PLACEMENT_3D('',#14620,#9828,#9829);
#8998=AXIS2_PLACEMENT_3D('',#14644,#9831,#9832);
#8999=AXIS2_PLACEMENT_3D('',#14669,#9834,#9835);
#9000=AXIS2_PLACEMENT_3D('',#14693,#9837,#9838);
#9001=AXIS2_PLACEMENT_3D('',#14718,#9840,#9841);
#9002=AXIS2_PLACEMENT_3D('',#14742,#9843,#9844);
#9003=AXIS2_PLACEMENT_3D('',#14767,#9846,#9847);
#9004=AXIS2_PLACEMENT_3D('',#14792,#9849,#9850);
#9005=AXIS2_PLACEMENT_3D('',#14816,#9852,#9853);
#9006=AXIS2_PLACEMENT_3D('',#14841,#9855,#9856);
#9007=AXIS2_PLACEMENT_3D('',#14865,#9858,#9859);
#9008=AXIS2_PLACEMENT_3D('',#14890,#9861,#9862);
#9009=AXIS2_PLACEMENT_3D('',#14914,#9864,#9865);
#9010=AXIS2_PLACEMENT_3D('',#14939,#9867,#9868);
#9011=AXIS2_PLACEMENT_3D('',#14964,#9870,#9871);
#9012=AXIS2_PLACEMENT_3D('',#14988,#9873,#9874);
#9013=AXIS2_PLACEMENT_3D('',#14999,#9876,#9877);
#9014=AXIS2_PLACEMENT_3D('',#15005,#9878,#9879);
#9015=AXIS2_PLACEMENT_3D('',#15015,#9881,#9882);
#9016=AXIS2_PLACEMENT_3D('',#15018,#9884,#9885);
#9017=AXIS2_PLACEMENT_3D('',#15020,#9886,#9887);
#9018=AXIS2_PLACEMENT_3D('',#15031,#9888,#9889);
#9019=AXIS2_PLACEMENT_3D('',#15079,#9891,#9892);
#9020=AXIS2_PLACEMENT_3D('',#15130,#9894,#9895);
#9021=AXIS2_PLACEMENT_3D('',#15178,#9897,#9898);
#9022=AXIS2_PLACEMENT_3D('',#15226,#9900,#9901);
#9023=AXIS2_PLACEMENT_3D('',#15277,#9903,#9904);
#9024=AXIS2_PLACEMENT_3D('',#15328,#9906,#9907);
#9025=AXIS2_PLACEMENT_3D('',#15376,#9909,#9910);
#9026=AXIS2_PLACEMENT_3D('',#15427,#9912,#9913);
#9027=AXIS2_PLACEMENT_3D('',#15478,#9915,#9916);
#9028=AXIS2_PLACEMENT_3D('',#15526,#9918,#9919);
#9029=AXIS2_PLACEMENT_3D('',#15574,#9921,#9922);
#9030=AXIS2_PLACEMENT_3D('',#15625,#9924,#9925);
#9031=AXIS2_PLACEMENT_3D('',#15676,#9927,#9928);
#9032=AXIS2_PLACEMENT_3D('',#15724,#9930,#9931);
#9033=AXIS2_PLACEMENT_3D('',#15775,#9933,#9934);
#9034=AXIS2_PLACEMENT_3D('',#15794,#9936,#9937);
#9035=AXIS2_PLACEMENT_3D('',#15814,#9938,#9939);
#9036=AXIS2_PLACEMENT_3D('',#15828,#9941,#9942);
#9037=AXIS2_PLACEMENT_3D('',#15838,#9943,#9944);
#9038=AXIS2_PLACEMENT_3D('',#15862,#9946,#9947);
#9039=AXIS2_PLACEMENT_3D('',#15887,#9949,#9950);
#9040=AXIS2_PLACEMENT_3D('',#15911,#9952,#9953);
#9041=AXIS2_PLACEMENT_3D('',#15936,#9955,#9956);
#9042=AXIS2_PLACEMENT_3D('',#15960,#9958,#9959);
#9043=AXIS2_PLACEMENT_3D('',#15985,#9961,#9962);
#9044=AXIS2_PLACEMENT_3D('',#16010,#9964,#9965);
#9045=AXIS2_PLACEMENT_3D('',#16034,#9967,#9968);
#9046=AXIS2_PLACEMENT_3D('',#16059,#9970,#9971);
#9047=AXIS2_PLACEMENT_3D('',#16083,#9973,#9974);
#9048=AXIS2_PLACEMENT_3D('',#16108,#9976,#9977);
#9049=AXIS2_PLACEMENT_3D('',#16132,#9979,#9980);
#9050=AXIS2_PLACEMENT_3D('',#16157,#9982,#9983);
#9051=AXIS2_PLACEMENT_3D('',#16182,#9985,#9986);
#9052=AXIS2_PLACEMENT_3D('',#16206,#9988,#9989);
#9053=AXIS2_PLACEMENT_3D('',#16217,#9991,#9992);
#9054=AXIS2_PLACEMENT_3D('',#16223,#9993,#9994);
#9055=AXIS2_PLACEMENT_3D('',#16406,#9995,#9996);
#9056=AXIS2_PLACEMENT_3D('',#17562,#9997,#9998);
#9057=AXIS2_PLACEMENT_3D('',#17563,#9999,#10000);
#9058=AXIS2_PLACEMENT_3D('',#17746,#10001,#10002);
#9059=AXIS2_PLACEMENT_3D('',#18902,#10003,#10004);
#9060=AXIS2_PLACEMENT_3D('',#18903,#10005,#10006);
#9061=AXIS2_PLACEMENT_3D('',#19086,#10007,#10008);
#9062=AXIS2_PLACEMENT_3D('',#20242,#10009,#10010);
#9063=AXIS2_PLACEMENT_3D('',#20243,#10011,#10012);
#9064=AXIS2_PLACEMENT_3D('',#20426,#10013,#10014);
#9065=AXIS2_PLACEMENT_3D('',#21582,#10015,#10016);
#9066=AXIS2_PLACEMENT_3D('',#21583,#10017,#10018);
#9067=AXIS2_PLACEMENT_3D('',#21584,#10019,#10020);
#9068=AXIS2_PLACEMENT_3D('',#21585,#10021,#10022);
#9069=AXIS2_PLACEMENT_3D('',#21586,#10023,#10024);
#9070=AXIS2_PLACEMENT_3D('',#21587,#10025,#10026);
#9071=AXIS2_PLACEMENT_3D('',#21596,#10031,#10032);
#9072=AXIS2_PLACEMENT_3D('',#21602,#10036,#10037);
#9073=AXIS2_PLACEMENT_3D('',#21608,#10041,#10042);
#9074=AXIS2_PLACEMENT_3D('',#21611,#10045,#10046);
#9075=AXIS2_PLACEMENT_3D('',#21620,#10051,#10052);
#9076=AXIS2_PLACEMENT_3D('',#21626,#10056,#10057);
#9077=AXIS2_PLACEMENT_3D('',#21632,#10061,#10062);
#9078=AXIS2_PLACEMENT_3D('',#21635,#10065,#10066);
#9079=AXIS2_PLACEMENT_3D('',#21636,#10067,#10068);
#9080=AXIS2_PLACEMENT_3D('',#21637,#10069,#10070);
#9081=AXIS2_PLACEMENT_3D('',#21638,#10071,#10072);
#9082=AXIS2_PLACEMENT_3D('',#21640,#10073,#10074);
#9083=AXIS2_PLACEMENT_3D('',#21643,#10076,#10077);
#9084=AXIS2_PLACEMENT_3D('',#21644,#10078,#10079);
#9085=AXIS2_PLACEMENT_3D('',#21646,#10080,#10081);
#9086=AXIS2_PLACEMENT_3D('',#21649,#10083,#10084);
#9087=AXIS2_PLACEMENT_3D('',#21650,#10085,#10086);
#9088=AXIS2_PLACEMENT_3D('',#21652,#10087,#10088);
#9089=AXIS2_PLACEMENT_3D('',#21655,#10090,#10091);
#9090=AXIS2_PLACEMENT_3D('',#21656,#10092,#10093);
#9091=AXIS2_PLACEMENT_3D('',#21658,#10094,#10095);
#9092=AXIS2_PLACEMENT_3D('',#21661,#10097,#10098);
#9093=AXIS2_PLACEMENT_3D('',#21662,#10099,#10100);
#9094=AXIS2_PLACEMENT_3D('',#21664,#10101,#10102);
#9095=AXIS2_PLACEMENT_3D('',#21667,#10104,#10105);
#9096=AXIS2_PLACEMENT_3D('',#21668,#10106,#10107);
#9097=AXIS2_PLACEMENT_3D('',#21677,#10112,#10113);
#9098=AXIS2_PLACEMENT_3D('',#21683,#10117,#10118);
#9099=AXIS2_PLACEMENT_3D('',#21689,#10122,#10123);
#9100=AXIS2_PLACEMENT_3D('',#21692,#10126,#10127);
#9101=AXIS2_PLACEMENT_3D('',#21693,#10128,#10129);
#9102=AXIS2_PLACEMENT_3D('',#21694,#10130,#10131);
#9103=AXIS2_PLACEMENT_3D('',#21695,#10132,#10133);
#9104=AXIS2_PLACEMENT_3D('',#21704,#10138,#10139);
#9105=AXIS2_PLACEMENT_3D('',#21710,#10143,#10144);
#9106=AXIS2_PLACEMENT_3D('',#21716,#10148,#10149);
#9107=AXIS2_PLACEMENT_3D('',#21719,#10152,#10153);
#9108=AXIS2_PLACEMENT_3D('',#21728,#10158,#10159);
#9109=AXIS2_PLACEMENT_3D('',#21734,#10163,#10164);
#9110=AXIS2_PLACEMENT_3D('',#21740,#10168,#10169);
#9111=AXIS2_PLACEMENT_3D('',#21743,#10172,#10173);
#9112=AXIS2_PLACEMENT_3D('',#21744,#10174,#10175);
#9113=AXIS2_PLACEMENT_3D('',#21745,#10176,#10177);
#9114=AXIS2_PLACEMENT_3D('',#21746,#10178,#10179);
#9115=AXIS2_PLACEMENT_3D('',#21771,#10181,#10182);
#9116=AXIS2_PLACEMENT_3D('',#21779,#10184,#10185);
#9117=AXIS2_PLACEMENT_3D('',#21802,#10186,#10187);
#9118=AXIS2_PLACEMENT_3D('',#21853,#10189,#10190);
#9119=AXIS2_PLACEMENT_3D('',#21901,#10192,#10193);
#9120=AXIS2_PLACEMENT_3D('',#21952,#10195,#10196);
#9121=AXIS2_PLACEMENT_3D('',#22003,#10198,#10199);
#9122=AXIS2_PLACEMENT_3D('',#22051,#10201,#10202);
#9123=AXIS2_PLACEMENT_3D('',#22099,#10204,#10205);
#9124=AXIS2_PLACEMENT_3D('',#22150,#10207,#10208);
#9125=AXIS2_PLACEMENT_3D('',#22198,#10210,#10211);
#9126=AXIS2_PLACEMENT_3D('',#22246,#10213,#10214);
#9127=AXIS2_PLACEMENT_3D('',#22297,#10216,#10217);
#9128=AXIS2_PLACEMENT_3D('',#22348,#10219,#10220);
#9129=AXIS2_PLACEMENT_3D('',#22396,#10222,#10223);
#9130=AXIS2_PLACEMENT_3D('',#22447,#10225,#10226);
#9131=AXIS2_PLACEMENT_3D('',#22466,#10228,#10229);
#9132=AXIS2_PLACEMENT_3D('',#22486,#10230,#10231);
#9133=AXIS2_PLACEMENT_3D('',#22498,#10233,#10234);
#9134=AXIS2_PLACEMENT_3D('',#22506,#10235,#10236);
#9135=AXIS2_PLACEMENT_3D('',#22530,#10238,#10239);
#9136=AXIS2_PLACEMENT_3D('',#22555,#10241,#10242);
#9137=AXIS2_PLACEMENT_3D('',#22580,#10244,#10245);
#9138=AXIS2_PLACEMENT_3D('',#22604,#10247,#10248);
#9139=AXIS2_PLACEMENT_3D('',#22629,#10250,#10251);
#9140=AXIS2_PLACEMENT_3D('',#22653,#10253,#10254);
#9141=AXIS2_PLACEMENT_3D('',#22678,#10256,#10257);
#9142=AXIS2_PLACEMENT_3D('',#22703,#10259,#10260);
#9143=AXIS2_PLACEMENT_3D('',#22727,#10262,#10263);
#9144=AXIS2_PLACEMENT_3D('',#22752,#10265,#10266);
#9145=AXIS2_PLACEMENT_3D('',#22776,#10268,#10269);
#9146=AXIS2_PLACEMENT_3D('',#22801,#10271,#10272);
#9147=AXIS2_PLACEMENT_3D('',#22826,#10274,#10275);
#9148=AXIS2_PLACEMENT_3D('',#22850,#10277,#10278);
#9149=AXIS2_PLACEMENT_3D('',#22861,#10280,#10281);
#9150=AXIS2_PLACEMENT_3D('',#22867,#10282,#10283);
#9151=AXIS2_PLACEMENT_3D('',#23041,#10284,#10285);
#9152=AXIS2_PLACEMENT_3D('',#24109,#10286,#10287);
#9153=AXIS2_PLACEMENT_3D('',#24110,#10288,#10289);
#9154=AXIS2_PLACEMENT_3D('',#24111,#10290,#10291);
#9155=AXIS2_PLACEMENT_3D('',#24120,#10296,#10297);
#9156=AXIS2_PLACEMENT_3D('',#24126,#10301,#10302);
#9157=AXIS2_PLACEMENT_3D('',#24132,#10306,#10307);
#9158=AXIS2_PLACEMENT_3D('',#24135,#10310,#10311);
#9159=AXIS2_PLACEMENT_3D('',#24136,#10312,#10313);
#9160=AXIS2_PLACEMENT_3D('',#24138,#10314,#10315);
#9161=AXIS2_PLACEMENT_3D('',#24141,#10317,#10318);
#9162=AXIS2_PLACEMENT_3D('',#24142,#10319,#10320);
#9163=AXIS2_PLACEMENT_3D('',#24144,#10321,#10322);
#9164=AXIS2_PLACEMENT_3D('',#24145,#10323,#10324);
#9165=AXIS2_PLACEMENT_3D('',#24147,#10325,#10326);
#9166=AXIS2_PLACEMENT_3D('',#24148,#10327,#10328);
#9167=AXIS2_PLACEMENT_3D('',#24150,#10329,#10330);
#9168=AXIS2_PLACEMENT_3D('',#24152,#10332,#10333);
#9169=AXIS2_PLACEMENT_3D('',#24161,#10338,#10339);
#9170=AXIS2_PLACEMENT_3D('',#24167,#10343,#10344);
#9171=AXIS2_PLACEMENT_3D('',#24173,#10348,#10349);
#9172=AXIS2_PLACEMENT_3D('',#24179,#10353,#10354);
#9173=AXIS2_PLACEMENT_3D('',#24185,#10358,#10359);
#9174=AXIS2_PLACEMENT_3D('',#24188,#10362,#10363);
#9175=AXIS2_PLACEMENT_3D('',#24189,#10364,#10365);
#9176=AXIS2_PLACEMENT_3D('',#24191,#10366,#10367);
#9177=AXIS2_PLACEMENT_3D('',#24193,#10368,#10369);
#9178=AXIS2_PLACEMENT_3D('',#24194,#10370,#10371);
#9179=AXIS2_PLACEMENT_3D('',#24197,#10373,#10374);
#9180=AXIS2_PLACEMENT_3D('',#24198,#10375,#10376);
#9181=AXIS2_PLACEMENT_3D('',#24199,#10377,#10378);
#9182=AXIS2_PLACEMENT_3D('',#24201,#10380,#10381);
#9183=AXIS2_PLACEMENT_3D('',#24202,#10382,#10383);
#9184=AXIS2_PLACEMENT_3D('',#24203,#10384,#10385);
#9185=AXIS2_PLACEMENT_3D('',#24212,#10390,#10391);
#9186=AXIS2_PLACEMENT_3D('',#24218,#10395,#10396);
#9187=AXIS2_PLACEMENT_3D('',#24224,#10400,#10401);
#9188=AXIS2_PLACEMENT_3D('',#24230,#10405,#10406);
#9189=AXIS2_PLACEMENT_3D('',#24236,#10410,#10411);
#9190=AXIS2_PLACEMENT_3D('',#24239,#10414,#10415);
#9191=AXIS2_PLACEMENT_3D('',#24248,#10420,#10421);
#9192=AXIS2_PLACEMENT_3D('',#24254,#10425,#10426);
#9193=AXIS2_PLACEMENT_3D('',#24260,#10430,#10431);
#9194=AXIS2_PLACEMENT_3D('',#24263,#10434,#10435);
#9195=AXIS2_PLACEMENT_3D('',#24264,#10436,#10437);
#9196=AXIS2_PLACEMENT_3D('',#24265,#10438,#10439);
#9197=AXIS2_PLACEMENT_3D('',#24266,#10440,#10441);
#9198=AXIS2_PLACEMENT_3D('',#24268,#10442,#10443);
#9199=AXIS2_PLACEMENT_3D('',#24271,#10445,#10446);
#9200=AXIS2_PLACEMENT_3D('',#24272,#10447,#10448);
#9201=AXIS2_PLACEMENT_3D('',#24274,#10449,#10450);
#9202=AXIS2_PLACEMENT_3D('',#24277,#10452,#10453);
#9203=AXIS2_PLACEMENT_3D('',#24278,#10454,#10455);
#9204=AXIS2_PLACEMENT_3D('',#24279,#10456,#10457);
#9205=AXIS2_PLACEMENT_3D('',#24280,#10458,#10459);
#9206=AXIS2_PLACEMENT_3D('',#24281,#10460,#10461);
#9207=AXIS2_PLACEMENT_3D('',#24290,#10466,#10467);
#9208=AXIS2_PLACEMENT_3D('',#24299,#10472,#10473);
#9209=AXIS2_PLACEMENT_3D('',#24300,#10474,#10475);
#9210=AXIS2_PLACEMENT_3D('',#24301,#10476,#10477);
#9211=AXIS2_PLACEMENT_3D('',#24302,#10478,#10479);
#9212=AXIS2_PLACEMENT_3D('',#24303,#10480,#10481);
#9213=AXIS2_PLACEMENT_3D('',#24304,#10482,#10483);
#9214=AXIS2_PLACEMENT_3D('',#24305,#10484,#10485);
#9215=AXIS2_PLACEMENT_3D('',#24306,#10486,#10487);
#9216=AXIS2_PLACEMENT_3D('',#24307,#10488,#10489);
#9217=AXIS2_PLACEMENT_3D('',#24308,#10490,#10491);
#9218=AXIS2_PLACEMENT_3D('',#24310,#10492,#10493);
#9219=AXIS2_PLACEMENT_3D('',#24313,#10495,#10496);
#9220=AXIS2_PLACEMENT_3D('',#24314,#10497,#10498);
#9221=AXIS2_PLACEMENT_3D('',#24316,#10499,#10500);
#9222=AXIS2_PLACEMENT_3D('',#24319,#10502,#10503);
#9223=AXIS2_PLACEMENT_3D('',#24320,#10504,#10505);
#9224=AXIS2_PLACEMENT_3D('',#24321,#10506,#10507);
#9225=AXIS2_PLACEMENT_3D('',#24322,#10508,#10509);
#9226=AXIS2_PLACEMENT_3D('',#24323,#10510,#10511);
#9227=AXIS2_PLACEMENT_3D('',#24339,#10513,#10514);
#9228=AXIS2_PLACEMENT_3D('',#24347,#10515,#10516);
#9229=AXIS2_PLACEMENT_3D('',#24395,#10518,#10519);
#9230=AXIS2_PLACEMENT_3D('',#24443,#10521,#10522);
#9231=AXIS2_PLACEMENT_3D('',#24494,#10524,#10525);
#9232=AXIS2_PLACEMENT_3D('',#24545,#10527,#10528);
#9233=AXIS2_PLACEMENT_3D('',#24593,#10530,#10531);
#9234=AXIS2_PLACEMENT_3D('',#24641,#10533,#10534);
#9235=AXIS2_PLACEMENT_3D('',#24695,#10536,#10537);
#9236=AXIS2_PLACEMENT_3D('',#24743,#10539,#10540);
#9237=AXIS2_PLACEMENT_3D('',#24791,#10542,#10543);
#9238=AXIS2_PLACEMENT_3D('',#24807,#10545,#10546);
#9239=AXIS2_PLACEMENT_3D('',#24816,#10547,#10548);
#9240=AXIS2_PLACEMENT_3D('',#24841,#10550,#10551);
#9241=AXIS2_PLACEMENT_3D('',#24865,#10553,#10554);
#9242=AXIS2_PLACEMENT_3D('',#24890,#10556,#10557);
#9243=AXIS2_PLACEMENT_3D('',#24915,#10559,#10560);
#9244=AXIS2_PLACEMENT_3D('',#24939,#10562,#10563);
#9245=AXIS2_PLACEMENT_3D('',#24963,#10565,#10566);
#9246=AXIS2_PLACEMENT_3D('',#24989,#10568,#10569);
#9247=AXIS2_PLACEMENT_3D('',#25013,#10571,#10572);
#9248=AXIS2_PLACEMENT_3D('',#25037,#10574,#10575);
#9249=AXIS2_PLACEMENT_3D('',#25304,#10576,#10577);
#9250=AXIS2_PLACEMENT_3D('',#25335,#10579,#10580);
#9251=AXIS2_PLACEMENT_3D('',#25729,#10581,#10582);
#9252=AXIS2_PLACEMENT_3D('',#25740,#10583,#10584);
#9253=AXIS2_PLACEMENT_3D('',#26133,#10585,#10586);
#9254=AXIS2_PLACEMENT_3D('',#26134,#10587,#10588);
#9255=AXIS2_PLACEMENT_3D('',#26143,#10593,#10594);
#9256=AXIS2_PLACEMENT_3D('',#26149,#10598,#10599);
#9257=AXIS2_PLACEMENT_3D('',#26155,#10603,#10604);
#9258=AXIS2_PLACEMENT_3D('',#26161,#10608,#10609);
#9259=AXIS2_PLACEMENT_3D('',#26167,#10613,#10614);
#9260=AXIS2_PLACEMENT_3D('',#26170,#10617,#10618);
#9261=AXIS2_PLACEMENT_3D('',#26171,#10619,#10620);
#9262=AXIS2_PLACEMENT_3D('',#26173,#10621,#10622);
#9263=AXIS2_PLACEMENT_3D('',#26174,#10623,#10624);
#9264=AXIS2_PLACEMENT_3D('',#26177,#10626,#10627);
#9265=AXIS2_PLACEMENT_3D('',#26178,#10628,#10629);
#9266=AXIS2_PLACEMENT_3D('',#26179,#10630,#10631);
#9267=AXIS2_PLACEMENT_3D('',#26180,#10632,#10633);
#9268=AXIS2_PLACEMENT_3D('',#26181,#10634,#10635);
#9269=AXIS2_PLACEMENT_3D('',#26190,#10640,#10641);
#9270=AXIS2_PLACEMENT_3D('',#26205,#10649,#10650);
#9271=AXIS2_PLACEMENT_3D('',#26207,#10651,#10652);
#9272=AXIS2_PLACEMENT_3D('',#26208,#10653,#10654);
#9273=AXIS2_PLACEMENT_3D('',#26211,#10656,#10657);
#9274=AXIS2_PLACEMENT_3D('',#26212,#10658,#10659);
#9275=AXIS2_PLACEMENT_3D('',#26215,#10661,#10662);
#9276=AXIS2_PLACEMENT_3D('',#26216,#10663,#10664);
#9277=AXIS2_PLACEMENT_3D('',#26220,#10666,#10667);
#9278=AXIS2_PLACEMENT_3D('',#26221,#10668,#10669);
#9279=AXIS2_PLACEMENT_3D('',#26222,#10670,#10671);
#9280=AXIS2_PLACEMENT_3D('',#26224,#10672,#10673);
#9281=AXIS2_PLACEMENT_3D('',#26227,#10675,#10676);
#9282=AXIS2_PLACEMENT_3D('',#26228,#10677,#10678);
#9283=AXIS2_PLACEMENT_3D('',#26230,#10680,#10681);
#9284=AXIS2_PLACEMENT_3D('',#26233,#10683,#10684);
#9285=AXIS2_PLACEMENT_3D('',#26235,#10685,#10686);
#9286=AXIS2_PLACEMENT_3D('',#26236,#10687,#10688);
#9287=AXIS2_PLACEMENT_3D('',#26239,#10690,#10691);
#9288=AXIS2_PLACEMENT_3D('',#26240,#10692,#10693);
#9289=AXIS2_PLACEMENT_3D('',#26243,#10695,#10696);
#9290=AXIS2_PLACEMENT_3D('',#26244,#10697,#10698);
#9291=AXIS2_PLACEMENT_3D('',#26248,#10701,#10702);
#9292=AXIS2_PLACEMENT_3D('',#26252,#10705,#10706);
#9293=AXIS2_PLACEMENT_3D('',#26254,#10708,#10709);
#9294=AXIS2_PLACEMENT_3D('',#26255,#10710,#10711);
#9295=AXIS2_PLACEMENT_3D('',#26256,#10712,#10713);
#9296=AXIS2_PLACEMENT_3D('',#26258,#10714,#10715);
#9297=AXIS2_PLACEMENT_3D('',#26261,#10717,#10718);
#9298=AXIS2_PLACEMENT_3D('',#26262,#10719,#10720);
#9299=AXIS2_PLACEMENT_3D('',#26264,#10721,#10722);
#9300=AXIS2_PLACEMENT_3D('',#26265,#10723,#10724);
#9301=AXIS2_PLACEMENT_3D('',#26267,#10725,#10726);
#9302=AXIS2_PLACEMENT_3D('',#26268,#10727,#10728);
#9303=AXIS2_PLACEMENT_3D('',#26270,#10729,#10730);
#9304=AXIS2_PLACEMENT_3D('',#26272,#10732,#10733);
#9305=AXIS2_PLACEMENT_3D('',#26274,#10734,#10735);
#9306=AXIS2_PLACEMENT_3D('',#26276,#10736,#10737);
#9307=AXIS2_PLACEMENT_3D('',#26277,#10738,#10739);
#9308=AXIS2_PLACEMENT_3D('',#26280,#10741,#10742);
#9309=AXIS2_PLACEMENT_3D('',#26281,#10743,#10744);
#9310=AXIS2_PLACEMENT_3D('',#26282,#10745,#10746);
#9311=AXIS2_PLACEMENT_3D('',#26284,#10748,#10749);
#9312=AXIS2_PLACEMENT_3D('',#26285,#10750,#10751);
#9313=AXIS2_PLACEMENT_3D('',#26286,#10752,#10753);
#9314=AXIS2_PLACEMENT_3D('',#26295,#10758,#10759);
#9315=AXIS2_PLACEMENT_3D('',#26304,#10764,#10765);
#9316=AXIS2_PLACEMENT_3D('',#26305,#10766,#10767);
#9317=AXIS2_PLACEMENT_3D('',#26306,#10768,#10769);
#9318=AXIS2_PLACEMENT_3D('',#26307,#10770,#10771);
#9319=AXIS2_PLACEMENT_3D('',#26308,#10772,#10773);
#9320=AXIS2_PLACEMENT_3D('',#26309,#10774,#10775);
#9321=AXIS2_PLACEMENT_3D('',#26310,#10776,#10777);
#9322=AXIS2_PLACEMENT_3D('',#26311,#10778,#10779);
#9323=AXIS2_PLACEMENT_3D('',#26312,#10780,#10781);
#9324=AXIS2_PLACEMENT_3D('',#26313,#10782,#10783);
#9325=AXIS2_PLACEMENT_3D('',#26322,#10788,#10789);
#9326=AXIS2_PLACEMENT_3D('',#26331,#10794,#10795);
#9327=AXIS2_PLACEMENT_3D('',#26343,#10802,#10803);
#9328=AXIS2_PLACEMENT_3D('',#26345,#10804,#10805);
#9329=AXIS2_PLACEMENT_3D('',#26346,#10806,#10807);
#9330=AXIS2_PLACEMENT_3D('',#26350,#10810,#10811);
#9331=AXIS2_PLACEMENT_3D('',#26352,#10812,#10813);
#9332=AXIS2_PLACEMENT_3D('',#26354,#10815,#10816);
#9333=AXIS2_PLACEMENT_3D('',#26356,#10817,#10818);
#9334=AXIS2_PLACEMENT_3D('',#26358,#10820,#10821);
#9335=AXIS2_PLACEMENT_3D('',#26360,#10822,#10823);
#9336=AXIS2_PLACEMENT_3D('',#26363,#10825,#10826);
#9337=AXIS2_PLACEMENT_3D('',#26364,#10827,#10828);
#9338=AXIS2_PLACEMENT_3D('',#26367,#10830,#10831);
#9339=AXIS2_PLACEMENT_3D('',#26368,#10832,#10833);
#9340=AXIS2_PLACEMENT_3D('',#26371,#10835,#10836);
#9341=AXIS2_PLACEMENT_3D('',#26372,#10837,#10838);
#9342=AXIS2_PLACEMENT_3D('',#26374,#10840,#10841);
#9343=AXIS2_PLACEMENT_3D('',#26378,#10844,#10845);
#9344=AXIS2_PLACEMENT_3D('',#26380,#10847,#10848);
#9345=AXIS2_PLACEMENT_3D('',#26381,#10849,#10850);
#9346=AXIS2_PLACEMENT_3D('',#26382,#10851,#10852);
#9347=AXIS2_PLACEMENT_3D('',#26384,#10853,#10854);
#9348=AXIS2_PLACEMENT_3D('',#26387,#10856,#10857);
#9349=AXIS2_PLACEMENT_3D('',#26388,#10858,#10859);
#9350=AXIS2_PLACEMENT_3D('',#26390,#10860,#10861);
#9351=AXIS2_PLACEMENT_3D('',#26393,#10863,#10864);
#9352=AXIS2_PLACEMENT_3D('',#26394,#10865,#10866);
#9353=AXIS2_PLACEMENT_3D('',#26395,#10867,#10868);
#9354=AXIS2_PLACEMENT_3D('',#26396,#10869,#10870);
#9355=AXIS2_PLACEMENT_3D('',#26397,#10871,#10872);
#9356=AXIS2_PLACEMENT_3D('',#26413,#10874,#10875);
#9357=AXIS2_PLACEMENT_3D('',#26421,#10876,#10877);
#9358=AXIS2_PLACEMENT_3D('',#26469,#10879,#10880);
#9359=AXIS2_PLACEMENT_3D('',#26517,#10882,#10883);
#9360=AXIS2_PLACEMENT_3D('',#26571,#10885,#10886);
#9361=AXIS2_PLACEMENT_3D('',#26619,#10888,#10889);
#9362=AXIS2_PLACEMENT_3D('',#26667,#10891,#10892);
#9363=AXIS2_PLACEMENT_3D('',#26721,#10894,#10895);
#9364=AXIS2_PLACEMENT_3D('',#26769,#10897,#10898);
#9365=AXIS2_PLACEMENT_3D('',#26817,#10900,#10901);
#9366=AXIS2_PLACEMENT_3D('',#26865,#10903,#10904);
#9367=AXIS2_PLACEMENT_3D('',#26919,#10906,#10907);
#9368=AXIS2_PLACEMENT_3D('',#26967,#10909,#10910);
#9369=AXIS2_PLACEMENT_3D('',#27015,#10912,#10913);
#9370=AXIS2_PLACEMENT_3D('',#27069,#10915,#10916);
#9371=AXIS2_PLACEMENT_3D('',#27117,#10918,#10919);
#9372=AXIS2_PLACEMENT_3D('',#27165,#10921,#10922);
#9373=AXIS2_PLACEMENT_3D('',#27219,#10924,#10925);
#9374=AXIS2_PLACEMENT_3D('',#27267,#10927,#10928);
#9375=AXIS2_PLACEMENT_3D('',#27315,#10930,#10931);
#9376=AXIS2_PLACEMENT_3D('',#27331,#10933,#10934);
#9377=AXIS2_PLACEMENT_3D('',#27340,#10935,#10936);
#9378=AXIS2_PLACEMENT_3D('',#27365,#10938,#10939);
#9379=AXIS2_PLACEMENT_3D('',#27389,#10941,#10942);
#9380=AXIS2_PLACEMENT_3D('',#27414,#10944,#10945);
#9381=AXIS2_PLACEMENT_3D('',#27439,#10947,#10948);
#9382=AXIS2_PLACEMENT_3D('',#27463,#10950,#10951);
#9383=AXIS2_PLACEMENT_3D('',#27488,#10953,#10954);
#9384=AXIS2_PLACEMENT_3D('',#27513,#10956,#10957);
#9385=AXIS2_PLACEMENT_3D('',#27537,#10959,#10960);
#9386=AXIS2_PLACEMENT_3D('',#27562,#10962,#10963);
#9387=AXIS2_PLACEMENT_3D('',#27587,#10965,#10966);
#9388=AXIS2_PLACEMENT_3D('',#27611,#10968,#10969);
#9389=AXIS2_PLACEMENT_3D('',#27635,#10971,#10972);
#9390=AXIS2_PLACEMENT_3D('',#27660,#10974,#10975);
#9391=AXIS2_PLACEMENT_3D('',#27685,#10977,#10978);
#9392=AXIS2_PLACEMENT_3D('',#27709,#10980,#10981);
#9393=AXIS2_PLACEMENT_3D('',#27734,#10983,#10984);
#9394=AXIS2_PLACEMENT_3D('',#27759,#10986,#10987);
#9395=AXIS2_PLACEMENT_3D('',#27783,#10989,#10990);
#9396=AXIS2_PLACEMENT_3D('',#28068,#10991,#10992);
#9397=AXIS2_PLACEMENT_3D('',#28102,#10994,#10995);
#9398=AXIS2_PLACEMENT_3D('',#28730,#10996,#10997);
#9399=AXIS2_PLACEMENT_3D('',#28741,#10998,#10999);
#9400=AXIS2_PLACEMENT_3D('',#29371,#11000,#11001);
#9401=AXIS2_PLACEMENT_3D('',#29372,#11002,#11003);
#9402=AXIS2_PLACEMENT_3D('',#29381,#11008,#11009);
#9403=AXIS2_PLACEMENT_3D('',#29387,#11013,#11014);
#9404=AXIS2_PLACEMENT_3D('',#29393,#11018,#11019);
#9405=AXIS2_PLACEMENT_3D('',#29399,#11023,#11024);
#9406=AXIS2_PLACEMENT_3D('',#29405,#11028,#11029);
#9407=AXIS2_PLACEMENT_3D('',#29408,#11032,#11033);
#9408=AXIS2_PLACEMENT_3D('',#29409,#11034,#11035);
#9409=AXIS2_PLACEMENT_3D('',#29411,#11036,#11037);
#9410=AXIS2_PLACEMENT_3D('',#29412,#11038,#11039);
#9411=AXIS2_PLACEMENT_3D('',#29415,#11041,#11042);
#9412=AXIS2_PLACEMENT_3D('',#29416,#11043,#11044);
#9413=AXIS2_PLACEMENT_3D('',#29417,#11045,#11046);
#9414=AXIS2_PLACEMENT_3D('',#29418,#11047,#11048);
#9415=AXIS2_PLACEMENT_3D('',#29419,#11049,#11050);
#9416=AXIS2_PLACEMENT_3D('',#29435,#11052,#11053);
#9417=AXIS2_PLACEMENT_3D('',#29443,#11054,#11055);
#9418=AXIS2_PLACEMENT_3D('',#29491,#11057,#11058);
#9419=AXIS2_PLACEMENT_3D('',#29539,#11060,#11061);
#9420=AXIS2_PLACEMENT_3D('',#29593,#11063,#11064);
#9421=AXIS2_PLACEMENT_3D('',#29641,#11066,#11067);
#9422=AXIS2_PLACEMENT_3D('',#29689,#11069,#11070);
#9423=AXIS2_PLACEMENT_3D('',#29743,#11072,#11073);
#9424=AXIS2_PLACEMENT_3D('',#29791,#11075,#11076);
#9425=AXIS2_PLACEMENT_3D('',#29842,#11078,#11079);
#9426=AXIS2_PLACEMENT_3D('',#29893,#11081,#11082);
#9427=AXIS2_PLACEMENT_3D('',#29941,#11084,#11085);
#9428=AXIS2_PLACEMENT_3D('',#29957,#11087,#11088);
#9429=AXIS2_PLACEMENT_3D('',#29966,#11089,#11090);
#9430=AXIS2_PLACEMENT_3D('',#29991,#11092,#11093);
#9431=AXIS2_PLACEMENT_3D('',#30015,#11095,#11096);
#9432=AXIS2_PLACEMENT_3D('',#30041,#11098,#11099);
#9433=AXIS2_PLACEMENT_3D('',#30065,#11101,#11102);
#9434=AXIS2_PLACEMENT_3D('',#30090,#11104,#11105);
#9435=AXIS2_PLACEMENT_3D('',#30115,#11107,#11108);
#9436=AXIS2_PLACEMENT_3D('',#30139,#11110,#11111);
#9437=AXIS2_PLACEMENT_3D('',#30164,#11113,#11114);
#9438=AXIS2_PLACEMENT_3D('',#30189,#11116,#11117);
#9439=AXIS2_PLACEMENT_3D('',#30213,#11119,#11120);
#9440=AXIS2_PLACEMENT_3D('',#30495,#11121,#11122);
#9441=AXIS2_PLACEMENT_3D('',#30529,#11124,#11125);
#9442=AXIS2_PLACEMENT_3D('',#30954,#11126,#11127);
#9443=AXIS2_PLACEMENT_3D('',#30965,#11128,#11129);
#9444=AXIS2_PLACEMENT_3D('',#31392,#11130,#11131);
#9445=AXIS2_PLACEMENT_3D('',#31393,#11132,#11133);
#9446=AXIS2_PLACEMENT_3D('',#31402,#11138,#11139);
#9447=AXIS2_PLACEMENT_3D('',#31408,#11143,#11144);
#9448=AXIS2_PLACEMENT_3D('',#31414,#11148,#11149);
#9449=AXIS2_PLACEMENT_3D('',#31420,#11153,#11154);
#9450=AXIS2_PLACEMENT_3D('',#31426,#11158,#11159);
#9451=AXIS2_PLACEMENT_3D('',#31429,#11162,#11163);
#9452=AXIS2_PLACEMENT_3D('',#31430,#11164,#11165);
#9453=AXIS2_PLACEMENT_3D('',#31432,#11166,#11167);
#9454=AXIS2_PLACEMENT_3D('',#31433,#11168,#11169);
#9455=AXIS2_PLACEMENT_3D('',#31436,#11171,#11172);
#9456=AXIS2_PLACEMENT_3D('',#31437,#11173,#11174);
#9457=AXIS2_PLACEMENT_3D('',#31438,#11175,#11176);
#9458=AXIS2_PLACEMENT_3D('',#31439,#11177,#11178);
#9459=AXIS2_PLACEMENT_3D('',#31440,#11179,#11180);
#9460=AXIS2_PLACEMENT_3D('',#31442,#11181,#11182);
#9461=AXIS2_PLACEMENT_3D('',#31445,#11184,#11185);
#9462=AXIS2_PLACEMENT_3D('',#31446,#11186,#11187);
#9463=AXIS2_PLACEMENT_3D('',#31448,#11188,#11189);
#9464=AXIS2_PLACEMENT_3D('',#31451,#11191,#11192);
#9465=AXIS2_PLACEMENT_3D('',#31452,#11193,#11194);
#9466=AXIS2_PLACEMENT_3D('',#31453,#11195,#11196);
#9467=AXIS2_PLACEMENT_3D('',#31454,#11197,#11198);
#9468=AXIS2_PLACEMENT_3D('',#31455,#11199,#11200);
#9469=AXIS2_PLACEMENT_3D('',#31465,#11202,#11203);
#9470=AXIS2_PLACEMENT_3D('',#31476,#11204,#11205);
#9471=AXIS2_PLACEMENT_3D('',#31527,#11207,#11208);
#9472=AXIS2_PLACEMENT_3D('',#31578,#11210,#11211);
#9473=AXIS2_PLACEMENT_3D('',#31626,#11213,#11214);
#9474=AXIS2_PLACEMENT_3D('',#31645,#11216,#11217);
#9475=AXIS2_PLACEMENT_3D('',#31665,#11218,#11219);
#9476=AXIS2_PLACEMENT_3D('',#31679,#11221,#11222);
#9477=AXIS2_PLACEMENT_3D('',#31689,#11223,#11224);
#9478=AXIS2_PLACEMENT_3D('',#31713,#11226,#11227);
#9479=AXIS2_PLACEMENT_3D('',#31738,#11229,#11230);
#9480=AXIS2_PLACEMENT_3D('',#31763,#11232,#11233);
#9481=AXIS2_PLACEMENT_3D('',#31774,#11235,#11236);
#9482=AXIS2_PLACEMENT_3D('',#31780,#11237,#11238);
#9483=AXIS2_PLACEMENT_3D('',#32512,#11239,#11240);
#9484=AXIS2_PLACEMENT_3D('',#32525,#11247,#11248);
#9485=AXIS2_PLACEMENT_3D('',#32526,#11249,#11250);
#9486=AXIS2_PLACEMENT_3D('',#32532,#11254,#11255);
#9487=AXIS2_PLACEMENT_3D('',#32536,#11258,#11259);
#9488=AXIS2_PLACEMENT_3D('',#32540,#11262,#11263);
#9489=AXIS2_PLACEMENT_3D('',#32544,#11266,#11267);
#9490=AXIS2_PLACEMENT_3D('',#32548,#11270,#11271);
#9491=AXIS2_PLACEMENT_3D('',#32550,#11273,#11274);
#9492=AXIS2_PLACEMENT_3D('',#32551,#11275,#11276);
#9493=AXIS2_PLACEMENT_3D('',#32552,#11277,#11278);
#9494=AXIS2_PLACEMENT_3D('',#32553,#11279,#11280);
#9495=AXIS2_PLACEMENT_3D('',#32554,#11281,#11282);
#9496=AXIS2_PLACEMENT_3D('',#32555,#11283,#11284);
#9497=AXIS2_PLACEMENT_3D('',#32556,#11285,#11286);
#9498=AXIS2_PLACEMENT_3D('',#32557,#11287,#11288);
#9499=AXIS2_PLACEMENT_3D('',#32558,#11289,#11290);
#9500=AXIS2_PLACEMENT_3D('',#32559,#11291,#11292);
#9501=AXIS2_PLACEMENT_3D('',#32560,#11293,#11294);
#9502=AXIS2_PLACEMENT_3D('',#32561,#11295,#11296);
#9503=AXIS2_PLACEMENT_3D('',#32562,#11297,#11298);
#9504=AXIS2_PLACEMENT_3D('',#32563,#11299,#11300);
#9505=AXIS2_PLACEMENT_3D('',#32564,#11301,#11302);
#9506=AXIS2_PLACEMENT_3D('',#32565,#11303,#11304);
#9507=AXIS2_PLACEMENT_3D('',#32566,#11305,#11306);
#9508=AXIS2_PLACEMENT_3D('',#32567,#11307,#11308);
#9509=AXIS2_PLACEMENT_3D('',#32568,#11309,#11310);
#9510=AXIS2_PLACEMENT_3D('',#32569,#11311,#11312);
#9511=AXIS2_PLACEMENT_3D('',#32570,#11313,#11314);
#9512=AXIS2_PLACEMENT_3D('',#32571,#11315,#11316);
#9513=AXIS2_PLACEMENT_3D('',#32572,#11317,#11318);
#9514=AXIS2_PLACEMENT_3D('',#32573,#11319,#11320);
#9515=AXIS2_PLACEMENT_3D('',#32574,#11321,#11322);
#9516=AXIS2_PLACEMENT_3D('',#32575,#11323,#11324);
#9517=AXIS2_PLACEMENT_3D('',#32576,#11325,#11326);
#9518=AXIS2_PLACEMENT_3D('',#32577,#11327,#11328);
#9519=AXIS2_PLACEMENT_3D('',#32578,#11329,#11330);
#9520=AXIS2_PLACEMENT_3D('',#32579,#11331,#11332);
#9521=AXIS2_PLACEMENT_3D('',#32580,#11333,#11334);
#9522=AXIS2_PLACEMENT_3D('',#32581,#11335,#11336);
#9523=AXIS2_PLACEMENT_3D('',#32582,#11337,#11338);
#9524=AXIS2_PLACEMENT_3D('',#32583,#11339,#11340);
#9525=AXIS2_PLACEMENT_3D('',#32584,#11341,#11342);
#9526=AXIS2_PLACEMENT_3D('',#32585,#11343,#11344);
#9527=AXIS2_PLACEMENT_3D('',#32586,#11345,#11346);
#9528=AXIS2_PLACEMENT_3D('',#32587,#11347,#11348);
#9529=DIRECTION('axis',(0.,0.,1.));
#9530=DIRECTION('refdir',(1.,0.,0.));
#9531=DIRECTION('axis',(0.,0.,1.));
#9532=DIRECTION('refdir',(1.,0.,0.));
#9533=DIRECTION('center_axis',(0.,0.,1.));
#9534=DIRECTION('ref_axis',(-1.,0.,0.));
#9535=DIRECTION('',(0.,0.,1.));
#9536=DIRECTION('center_axis',(0.,0.,-1.));
#9537=DIRECTION('ref_axis',(-1.,0.,0.));
#9538=DIRECTION('',(0.,0.,1.));
#9539=DIRECTION('center_axis',(0.,0.,-1.));
#9540=DIRECTION('ref_axis',(-1.,0.,0.));
#9541=DIRECTION('center_axis',(0.,0.,-1.));
#9542=DIRECTION('ref_axis',(-1.,0.,0.));
#9543=DIRECTION('center_axis',(0.,0.,1.));
#9544=DIRECTION('ref_axis',(-1.,0.,0.));
#9545=DIRECTION('',(0.,0.,1.));
#9546=DIRECTION('center_axis',(0.,0.,1.));
#9547=DIRECTION('ref_axis',(-1.,0.,0.));
#9548=DIRECTION('',(0.,0.,1.));
#9549=DIRECTION('center_axis',(0.,0.,1.));
#9550=DIRECTION('ref_axis',(-1.,0.,0.));
#9551=DIRECTION('',(0.,0.,1.));
#9552=DIRECTION('center_axis',(0.,0.,1.));
#9553=DIRECTION('ref_axis',(-1.,0.,0.));
#9554=DIRECTION('',(0.,0.,1.));
#9555=DIRECTION('center_axis',(0.,0.,1.));
#9556=DIRECTION('ref_axis',(-1.,0.,0.));
#9557=DIRECTION('',(0.,0.,1.));
#9558=DIRECTION('center_axis',(0.,0.,1.));
#9559=DIRECTION('ref_axis',(-1.,0.,0.));
#9560=DIRECTION('',(0.,0.,1.));
#9561=DIRECTION('center_axis',(0.,0.,1.));
#9562=DIRECTION('ref_axis',(-1.,0.,0.));
#9563=DIRECTION('',(0.,0.,1.));
#9564=DIRECTION('center_axis',(0.,0.,1.));
#9565=DIRECTION('ref_axis',(-1.,0.,0.));
#9566=DIRECTION('',(0.,0.,1.));
#9567=DIRECTION('center_axis',(0.,0.,1.));
#9568=DIRECTION('ref_axis',(-1.,0.,0.));
#9569=DIRECTION('',(0.,0.,1.));
#9570=DIRECTION('center_axis',(0.,0.,1.));
#9571=DIRECTION('ref_axis',(-1.,0.,0.));
#9572=DIRECTION('',(0.,0.,1.));
#9573=DIRECTION('center_axis',(0.,0.,1.));
#9574=DIRECTION('ref_axis',(-1.,0.,0.));
#9575=DIRECTION('',(0.,0.,1.));
#9576=DIRECTION('center_axis',(0.,0.,1.));
#9577=DIRECTION('ref_axis',(-1.,0.,0.));
#9578=DIRECTION('',(0.,0.,1.));
#9579=DIRECTION('center_axis',(0.,0.,1.));
#9580=DIRECTION('ref_axis',(-1.,0.,0.));
#9581=DIRECTION('',(0.,0.,1.));
#9582=DIRECTION('center_axis',(0.,0.,1.));
#9583=DIRECTION('ref_axis',(-1.,0.,0.));
#9584=DIRECTION('',(0.,0.,1.));
#9585=DIRECTION('center_axis',(0.,0.,1.));
#9586=DIRECTION('ref_axis',(-1.,0.,0.));
#9587=DIRECTION('',(0.,0.,1.));
#9588=DIRECTION('center_axis',(0.,0.,1.));
#9589=DIRECTION('ref_axis',(-0.937990746613933,-0.34666029375548,0.));
#9590=DIRECTION('',(0.,0.,1.));
#9591=DIRECTION('center_axis',(0.,0.,-1.));
#9592=DIRECTION('ref_axis',(-1.,0.,0.));
#9593=DIRECTION('center_axis',(0.,0.,1.));
#9594=DIRECTION('ref_axis',(-1.,-9.82530218636873E-14,0.));
#9595=DIRECTION('',(-1.22464679914735E-16,-1.20475224710186E-29,1.));
#9596=DIRECTION('center_axis',(0.,0.,-1.));
#9597=DIRECTION('ref_axis',(-1.,-9.82530218636873E-14,0.));
#9598=DIRECTION('center_axis',(0.,0.,1.));
#9599=DIRECTION('ref_axis',(-1.,-9.82530218636873E-14,0.));
#9600=DIRECTION('',(-1.22464679914735E-16,-1.20475224710186E-29,1.));
#9601=DIRECTION('center_axis',(0.,0.,1.));
#9602=DIRECTION('ref_axis',(-1.,-9.82530218636873E-14,0.));
#9603=DIRECTION('',(-1.22464679914735E-16,-1.20475224710186E-29,1.));
#9604=DIRECTION('center_axis',(0.,0.,1.));
#9605=DIRECTION('ref_axis',(-1.,-9.82530218636873E-14,0.));
#9606=DIRECTION('',(-1.22464679914735E-16,-1.20475224710186E-29,1.));
#9607=DIRECTION('center_axis',(0.,0.,1.));
#9608=DIRECTION('ref_axis',(-1.,-9.82530218636873E-14,0.));
#9609=DIRECTION('',(-1.22464679914735E-16,-1.20475224710186E-29,1.));
#9610=DIRECTION('center_axis',(0.,0.,1.));
#9611=DIRECTION('ref_axis',(-1.,-9.82530218636873E-14,0.));
#9612=DIRECTION('',(-1.22464679914735E-16,-1.20475224710186E-29,1.));
#9613=DIRECTION('center_axis',(0.,0.,1.));
#9614=DIRECTION('ref_axis',(-1.,-9.82530218636873E-14,0.));
#9615=DIRECTION('',(-1.22464679914735E-16,-1.20475224710186E-29,1.));
#9616=DIRECTION('center_axis',(0.,0.,1.));
#9617=DIRECTION('ref_axis',(-1.,-9.82530218636873E-14,0.));
#9618=DIRECTION('',(-1.22464679914735E-16,-1.20475224710186E-29,1.));
#9619=DIRECTION('center_axis',(0.,0.,1.));
#9620=DIRECTION('ref_axis',(-1.,-9.82530218636873E-14,0.));
#9621=DIRECTION('',(-1.22464679914735E-16,-1.20475224710186E-29,1.));
#9622=DIRECTION('center_axis',(0.,0.,1.));
#9623=DIRECTION('ref_axis',(-1.,-9.82530218636873E-14,0.));
#9624=DIRECTION('',(-1.22464679914735E-16,-1.20475224710186E-29,1.));
#9625=DIRECTION('center_axis',(0.,0.,1.));
#9626=DIRECTION('ref_axis',(-1.,-9.82530218636873E-14,0.));
#9627=DIRECTION('',(-1.22464679914735E-16,-1.20475224710186E-29,1.));
#9628=DIRECTION('center_axis',(0.,0.,1.));
#9629=DIRECTION('ref_axis',(-1.,-9.82530218636873E-14,0.));
#9630=DIRECTION('',(-1.22464679914735E-16,-1.20475224710186E-29,1.));
#9631=DIRECTION('center_axis',(0.,0.,1.));
#9632=DIRECTION('ref_axis',(-1.,-9.82530218636873E-14,0.));
#9633=DIRECTION('',(-1.22464679914735E-16,-1.20475224710186E-29,1.));
#9634=DIRECTION('center_axis',(0.,0.,1.));
#9635=DIRECTION('ref_axis',(-1.,-9.82530218636873E-14,0.));
#9636=DIRECTION('',(-1.22464679914735E-16,-1.20475224710186E-29,1.));
#9637=DIRECTION('center_axis',(0.,0.,1.));
#9638=DIRECTION('ref_axis',(-1.,-9.82530218636873E-14,0.));
#9639=DIRECTION('',(-1.22464679914735E-16,-1.20475224710186E-29,1.));
#9640=DIRECTION('center_axis',(0.,0.,1.));
#9641=DIRECTION('ref_axis',(-1.,-9.82530218636873E-14,0.));
#9642=DIRECTION('',(-1.22464679914735E-16,-1.20475224710186E-29,1.));
#9643=DIRECTION('center_axis',(0.,0.,1.));
#9644=DIRECTION('ref_axis',(0.60923771710773,-0.792987644325787,0.));
#9645=DIRECTION('',(-1.22464679914735E-16,-1.20475224710186E-29,1.));
#9646=DIRECTION('center_axis',(0.,0.,1.));
#9647=DIRECTION('ref_axis',(-1.,-9.82530218636873E-14,0.));
#9648=DIRECTION('center_axis',(0.,0.,1.));
#9649=DIRECTION('ref_axis',(-1.,0.,0.));
#9650=DIRECTION('',(0.,0.,1.));
#9651=DIRECTION('center_axis',(0.,0.,-1.));
#9652=DIRECTION('ref_axis',(-1.,0.,0.));
#9653=DIRECTION('',(0.,0.,1.));
#9654=DIRECTION('center_axis',(0.,0.,-1.));
#9655=DIRECTION('ref_axis',(-1.,0.,0.));
#9656=DIRECTION('center_axis',(0.,0.,-1.));
#9657=DIRECTION('ref_axis',(-1.,0.,0.));
#9658=DIRECTION('center_axis',(0.,0.,1.));
#9659=DIRECTION('ref_axis',(-1.,0.,0.));
#9660=DIRECTION('',(0.,0.,1.));
#9661=DIRECTION('center_axis',(0.,0.,1.));
#9662=DIRECTION('ref_axis',(-1.,0.,0.));
#9663=DIRECTION('',(0.,0.,1.));
#9664=DIRECTION('center_axis',(0.,0.,1.));
#9665=DIRECTION('ref_axis',(-1.,0.,0.));
#9666=DIRECTION('',(0.,0.,1.));
#9667=DIRECTION('center_axis',(0.,0.,1.));
#9668=DIRECTION('ref_axis',(-1.,0.,0.));
#9669=DIRECTION('',(0.,0.,1.));
#9670=DIRECTION('center_axis',(0.,0.,1.));
#9671=DIRECTION('ref_axis',(-1.,0.,0.));
#9672=DIRECTION('',(0.,0.,1.));
#9673=DIRECTION('center_axis',(0.,0.,1.));
#9674=DIRECTION('ref_axis',(-1.,0.,0.));
#9675=DIRECTION('',(0.,0.,1.));
#9676=DIRECTION('center_axis',(0.,0.,1.));
#9677=DIRECTION('ref_axis',(-1.,0.,0.));
#9678=DIRECTION('',(0.,0.,1.));
#9679=DIRECTION('center_axis',(0.,0.,1.));
#9680=DIRECTION('ref_axis',(-1.,0.,0.));
#9681=DIRECTION('',(0.,0.,1.));
#9682=DIRECTION('center_axis',(0.,0.,1.));
#9683=DIRECTION('ref_axis',(-1.,0.,0.));
#9684=DIRECTION('',(0.,0.,1.));
#9685=DIRECTION('center_axis',(0.,0.,1.));
#9686=DIRECTION('ref_axis',(-1.,0.,0.));
#9687=DIRECTION('',(0.,0.,1.));
#9688=DIRECTION('center_axis',(0.,0.,1.));
#9689=DIRECTION('ref_axis',(-1.,0.,0.));
#9690=DIRECTION('',(0.,0.,1.));
#9691=DIRECTION('center_axis',(0.,0.,1.));
#9692=DIRECTION('ref_axis',(-1.,0.,0.));
#9693=DIRECTION('',(0.,0.,1.));
#9694=DIRECTION('center_axis',(0.,0.,1.));
#9695=DIRECTION('ref_axis',(-1.,0.,0.));
#9696=DIRECTION('',(0.,0.,1.));
#9697=DIRECTION('center_axis',(0.,0.,1.));
#9698=DIRECTION('ref_axis',(-1.,0.,0.));
#9699=DIRECTION('',(0.,0.,1.));
#9700=DIRECTION('center_axis',(0.,0.,1.));
#9701=DIRECTION('ref_axis',(-1.,0.,0.));
#9702=DIRECTION('',(0.,0.,1.));
#9703=DIRECTION('center_axis',(0.,0.,1.));
#9704=DIRECTION('ref_axis',(-0.937990745316897,-0.346660297264991,0.));
#9705=DIRECTION('',(0.,0.,1.));
#9706=DIRECTION('center_axis',(0.,0.,-1.));
#9707=DIRECTION('ref_axis',(-1.,0.,0.));
#9708=DIRECTION('center_axis',(0.,0.,1.));
#9709=DIRECTION('ref_axis',(-1.,-1.09812200906474E-13,0.));
#9710=DIRECTION('',(-1.22464679914735E-16,-1.34631136325706E-29,1.));
#9711=DIRECTION('center_axis',(0.,0.,-1.));
#9712=DIRECTION('ref_axis',(-1.,-1.09812200906474E-13,0.));
#9713=DIRECTION('center_axis',(0.,0.,1.));
#9714=DIRECTION('ref_axis',(-1.,-1.09812200906474E-13,0.));
#9715=DIRECTION('',(-1.22464679914735E-16,-1.34631136325706E-29,1.));
#9716=DIRECTION('center_axis',(0.,0.,1.));
#9717=DIRECTION('ref_axis',(-1.,-1.09812200906474E-13,0.));
#9718=DIRECTION('',(-1.22464679914735E-16,-1.34631136325706E-29,1.));
#9719=DIRECTION('center_axis',(0.,0.,1.));
#9720=DIRECTION('ref_axis',(-1.,-1.09812200906474E-13,0.));
#9721=DIRECTION('',(-1.22464679914735E-16,-1.34631136325706E-29,1.));
#9722=DIRECTION('center_axis',(0.,0.,1.));
#9723=DIRECTION('ref_axis',(-1.,-1.09812200906474E-13,0.));
#9724=DIRECTION('',(-1.22464679914735E-16,-1.34631136325706E-29,1.));
#9725=DIRECTION('center_axis',(0.,0.,1.));
#9726=DIRECTION('ref_axis',(-1.,-1.09812200906474E-13,0.));
#9727=DIRECTION('',(-1.22464679914735E-16,-1.34631136325706E-29,1.));
#9728=DIRECTION('center_axis',(0.,0.,1.));
#9729=DIRECTION('ref_axis',(-1.,-1.09812200906474E-13,0.));
#9730=DIRECTION('',(-1.22464679914735E-16,-1.34631136325706E-29,1.));
#9731=DIRECTION('center_axis',(0.,0.,1.));
#9732=DIRECTION('ref_axis',(-1.,-1.09812200906474E-13,0.));
#9733=DIRECTION('',(-1.22464679914735E-16,-1.34631136325706E-29,1.));
#9734=DIRECTION('center_axis',(0.,0.,1.));
#9735=DIRECTION('ref_axis',(-1.,-1.09812200906474E-13,0.));
#9736=DIRECTION('',(-1.22464679914735E-16,-1.34631136325706E-29,1.));
#9737=DIRECTION('center_axis',(0.,0.,1.));
#9738=DIRECTION('ref_axis',(-1.,-1.09812200906474E-13,0.));
#9739=DIRECTION('',(-1.22464679914735E-16,-1.34631136325706E-29,1.));
#9740=DIRECTION('center_axis',(0.,0.,1.));
#9741=DIRECTION('ref_axis',(-1.,-1.09812200906474E-13,0.));
#9742=DIRECTION('',(-1.22464679914735E-16,-1.34631136325706E-29,1.));
#9743=DIRECTION('center_axis',(0.,0.,1.));
#9744=DIRECTION('ref_axis',(-1.,-1.09812200906474E-13,0.));
#9745=DIRECTION('',(-1.22464679914735E-16,-1.34631136325706E-29,1.));
#9746=DIRECTION('center_axis',(0.,0.,1.));
#9747=DIRECTION('ref_axis',(-1.,-1.09812200906474E-13,0.));
#9748=DIRECTION('',(-1.22464679914735E-16,-1.34631136325706E-29,1.));
#9749=DIRECTION('center_axis',(0.,0.,1.));
#9750=DIRECTION('ref_axis',(-1.,-1.09812200906474E-13,0.));
#9751=DIRECTION('',(-1.22464679914735E-16,-1.34631136325706E-29,1.));
#9752=DIRECTION('center_axis',(0.,0.,1.));
#9753=DIRECTION('ref_axis',(-1.,-1.09812200906474E-13,0.));
#9754=DIRECTION('',(-1.22464679914735E-16,-1.34631136325706E-29,1.));
#9755=DIRECTION('center_axis',(0.,0.,1.));
#9756=DIRECTION('ref_axis',(-1.,-1.09812200906474E-13,0.));
#9757=DIRECTION('',(-1.22464679914735E-16,-1.34631136325706E-29,1.));
#9758=DIRECTION('center_axis',(0.,0.,1.));
#9759=DIRECTION('ref_axis',(0.609237720020655,-0.792987642087841,0.));
#9760=DIRECTION('',(-1.22464679914735E-16,-1.34631136325706E-29,1.));
#9761=DIRECTION('center_axis',(0.,0.,1.));
#9762=DIRECTION('ref_axis',(-1.,-1.09812200906474E-13,0.));
#9763=DIRECTION('center_axis',(0.,0.,1.));
#9764=DIRECTION('ref_axis',(-1.,0.,0.));
#9765=DIRECTION('',(0.,0.,1.));
#9766=DIRECTION('center_axis',(0.,0.,-1.));
#9767=DIRECTION('ref_axis',(-1.,0.,0.));
#9768=DIRECTION('',(0.,0.,1.));
#9769=DIRECTION('center_axis',(0.,0.,-1.));
#9770=DIRECTION('ref_axis',(-1.,0.,0.));
#9771=DIRECTION('center_axis',(0.,0.,-1.));
#9772=DIRECTION('ref_axis',(-1.,0.,0.));
#9773=DIRECTION('center_axis',(0.,0.,1.));
#9774=DIRECTION('ref_axis',(-1.,0.,0.));
#9775=DIRECTION('',(0.,0.,1.));
#9776=DIRECTION('center_axis',(0.,0.,1.));
#9777=DIRECTION('ref_axis',(-1.,0.,0.));
#9778=DIRECTION('',(0.,0.,1.));
#9779=DIRECTION('center_axis',(0.,0.,1.));
#9780=DIRECTION('ref_axis',(-1.,0.,0.));
#9781=DIRECTION('',(0.,0.,1.));
#9782=DIRECTION('center_axis',(0.,0.,1.));
#9783=DIRECTION('ref_axis',(-1.,0.,0.));
#9784=DIRECTION('',(0.,0.,1.));
#9785=DIRECTION('center_axis',(0.,0.,1.));
#9786=DIRECTION('ref_axis',(-1.,0.,0.));
#9787=DIRECTION('',(0.,0.,1.));
#9788=DIRECTION('center_axis',(0.,0.,1.));
#9789=DIRECTION('ref_axis',(-1.,0.,0.));
#9790=DIRECTION('',(0.,0.,1.));
#9791=DIRECTION('center_axis',(0.,0.,1.));
#9792=DIRECTION('ref_axis',(-1.,0.,0.));
#9793=DIRECTION('',(0.,0.,1.));
#9794=DIRECTION('center_axis',(0.,0.,1.));
#9795=DIRECTION('ref_axis',(-1.,0.,0.));
#9796=DIRECTION('',(0.,0.,1.));
#9797=DIRECTION('center_axis',(0.,0.,1.));
#9798=DIRECTION('ref_axis',(-1.,0.,0.));
#9799=DIRECTION('',(0.,0.,1.));
#9800=DIRECTION('center_axis',(0.,0.,1.));
#9801=DIRECTION('ref_axis',(-1.,0.,0.));
#9802=DIRECTION('',(0.,0.,1.));
#9803=DIRECTION('center_axis',(0.,0.,1.));
#9804=DIRECTION('ref_axis',(-1.,0.,0.));
#9805=DIRECTION('',(0.,0.,1.));
#9806=DIRECTION('center_axis',(0.,0.,1.));
#9807=DIRECTION('ref_axis',(-1.,0.,0.));
#9808=DIRECTION('',(0.,0.,1.));
#9809=DIRECTION('center_axis',(0.,0.,1.));
#9810=DIRECTION('ref_axis',(-1.,0.,0.));
#9811=DIRECTION('',(0.,0.,1.));
#9812=DIRECTION('center_axis',(0.,0.,1.));
#9813=DIRECTION('ref_axis',(-1.,0.,0.));
#9814=DIRECTION('',(0.,0.,1.));
#9815=DIRECTION('center_axis',(0.,0.,1.));
#9816=DIRECTION('ref_axis',(-1.,0.,0.));
#9817=DIRECTION('',(0.,0.,1.));
#9818=DIRECTION('center_axis',(0.,0.,1.));
#9819=DIRECTION('ref_axis',(-0.937990855083185,-0.346660000260074,0.));
#9820=DIRECTION('',(0.,0.,1.));
#9821=DIRECTION('center_axis',(0.,0.,-1.));
#9822=DIRECTION('ref_axis',(-1.,0.,0.));
#9823=DIRECTION('center_axis',(0.,0.,1.));
#9824=DIRECTION('ref_axis',(-1.,-1.01142816624385E-13,0.));
#9825=DIRECTION('',(-1.22464679914735E-16,-1.24014202614067E-29,1.));
#9826=DIRECTION('center_axis',(0.,0.,-1.));
#9827=DIRECTION('ref_axis',(-1.,-1.01142816624385E-13,0.));
#9828=DIRECTION('center_axis',(0.,0.,1.));
#9829=DIRECTION('ref_axis',(-1.,-1.01142816624385E-13,0.));
#9830=DIRECTION('',(-1.22464679914735E-16,-1.24014202614067E-29,1.));
#9831=DIRECTION('center_axis',(0.,0.,1.));
#9832=DIRECTION('ref_axis',(-1.,-1.01142816624385E-13,0.));
#9833=DIRECTION('',(-1.22464679914735E-16,-1.24014202614067E-29,1.));
#9834=DIRECTION('center_axis',(0.,0.,1.));
#9835=DIRECTION('ref_axis',(-1.,-1.01142816624385E-13,0.));
#9836=DIRECTION('',(-1.22464679914735E-16,-1.24014202614067E-29,1.));
#9837=DIRECTION('center_axis',(0.,0.,1.));
#9838=DIRECTION('ref_axis',(-1.,-1.01142816624385E-13,0.));
#9839=DIRECTION('',(-1.22464679914735E-16,-1.24014202614067E-29,1.));
#9840=DIRECTION('center_axis',(0.,0.,1.));
#9841=DIRECTION('ref_axis',(-1.,-1.01142816624385E-13,0.));
#9842=DIRECTION('',(-1.22464679914735E-16,-1.24014202614067E-29,1.));
#9843=DIRECTION('center_axis',(0.,0.,1.));
#9844=DIRECTION('ref_axis',(-1.,-1.01142816624385E-13,0.));
#9845=DIRECTION('',(-1.22464679914735E-16,-1.24014202614067E-29,1.));
#9846=DIRECTION('center_axis',(0.,0.,1.));
#9847=DIRECTION('ref_axis',(-1.,-1.01142816624385E-13,0.));
#9848=DIRECTION('',(-1.22464679914735E-16,-1.24014202614067E-29,1.));
#9849=DIRECTION('center_axis',(0.,0.,1.));
#9850=DIRECTION('ref_axis',(-1.,-1.01142816624385E-13,0.));
#9851=DIRECTION('',(-1.22464679914735E-16,-1.24014202614067E-29,1.));
#9852=DIRECTION('center_axis',(0.,0.,1.));
#9853=DIRECTION('ref_axis',(-1.,-1.01142816624385E-13,0.));
#9854=DIRECTION('',(-1.22464679914735E-16,-1.24014202614067E-29,1.));
#9855=DIRECTION('center_axis',(0.,0.,1.));
#9856=DIRECTION('ref_axis',(-1.,-1.01142816624385E-13,0.));
#9857=DIRECTION('',(-1.22464679914735E-16,-1.24014202614067E-29,1.));
#9858=DIRECTION('center_axis',(0.,0.,1.));
#9859=DIRECTION('ref_axis',(-1.,-1.01142816624385E-13,0.));
#9860=DIRECTION('',(-1.22464679914735E-16,-1.24014202614067E-29,1.));
#9861=DIRECTION('center_axis',(0.,0.,1.));
#9862=DIRECTION('ref_axis',(-1.,-1.01142816624385E-13,0.));
#9863=DIRECTION('',(-1.22464679914735E-16,-1.24014202614067E-29,1.));
#9864=DIRECTION('center_axis',(0.,0.,1.));
#9865=DIRECTION('ref_axis',(-1.,-1.01142816624385E-13,0.));
#9866=DIRECTION('',(-1.22464679914735E-16,-1.24014202614067E-29,1.));
#9867=DIRECTION('center_axis',(0.,0.,1.));
#9868=DIRECTION('ref_axis',(-1.,-1.01142816624385E-13,0.));
#9869=DIRECTION('',(-1.22464679914735E-16,-1.24014202614067E-29,1.));
#9870=DIRECTION('center_axis',(0.,0.,1.));
#9871=DIRECTION('ref_axis',(-1.,-1.01142816624385E-13,0.));
#9872=DIRECTION('',(-1.22464679914735E-16,-1.24014202614067E-29,1.));
#9873=DIRECTION('center_axis',(0.,0.,1.));
#9874=DIRECTION('ref_axis',(0.609237468266457,-0.792987835505865,0.));
#9875=DIRECTION('',(-1.22464679914735E-16,-1.24014202614067E-29,1.));
#9876=DIRECTION('center_axis',(0.,0.,1.));
#9877=DIRECTION('ref_axis',(-1.,-1.01142816624385E-13,0.));
#9878=DIRECTION('center_axis',(0.,0.,1.));
#9879=DIRECTION('ref_axis',(-1.,0.,0.));
#9880=DIRECTION('',(0.,0.,1.));
#9881=DIRECTION('center_axis',(0.,0.,-1.));
#9882=DIRECTION('ref_axis',(-1.,0.,0.));
#9883=DIRECTION('',(0.,0.,1.));
#9884=DIRECTION('center_axis',(0.,0.,-1.));
#9885=DIRECTION('ref_axis',(-1.,0.,0.));
#9886=DIRECTION('center_axis',(0.,0.,-1.));
#9887=DIRECTION('ref_axis',(-1.,0.,0.));
#9888=DIRECTION('center_axis',(0.,0.,1.));
#9889=DIRECTION('ref_axis',(-1.,0.,0.));
#9890=DIRECTION('',(0.,0.,1.));
#9891=DIRECTION('center_axis',(0.,0.,1.));
#9892=DIRECTION('ref_axis',(-1.,0.,0.));
#9893=DIRECTION('',(0.,0.,1.));
#9894=DIRECTION('center_axis',(0.,0.,1.));
#9895=DIRECTION('ref_axis',(-1.,0.,0.));
#9896=DIRECTION('',(0.,0.,1.));
#9897=DIRECTION('center_axis',(0.,0.,1.));
#9898=DIRECTION('ref_axis',(-1.,0.,0.));
#9899=DIRECTION('',(0.,0.,1.));
#9900=DIRECTION('center_axis',(0.,0.,1.));
#9901=DIRECTION('ref_axis',(-1.,0.,0.));
#9902=DIRECTION('',(0.,0.,1.));
#9903=DIRECTION('center_axis',(0.,0.,1.));
#9904=DIRECTION('ref_axis',(-1.,0.,0.));
#9905=DIRECTION('',(0.,0.,1.));
#9906=DIRECTION('center_axis',(0.,0.,1.));
#9907=DIRECTION('ref_axis',(-1.,0.,0.));
#9908=DIRECTION('',(0.,0.,1.));
#9909=DIRECTION('center_axis',(0.,0.,1.));
#9910=DIRECTION('ref_axis',(-1.,0.,0.));
#9911=DIRECTION('',(0.,0.,1.));
#9912=DIRECTION('center_axis',(0.,0.,1.));
#9913=DIRECTION('ref_axis',(-1.,0.,0.));
#9914=DIRECTION('',(0.,0.,1.));
#9915=DIRECTION('center_axis',(0.,0.,1.));
#9916=DIRECTION('ref_axis',(-1.,0.,0.));
#9917=DIRECTION('',(0.,0.,1.));
#9918=DIRECTION('center_axis',(0.,0.,1.));
#9919=DIRECTION('ref_axis',(-1.,0.,0.));
#9920=DIRECTION('',(0.,0.,1.));
#9921=DIRECTION('center_axis',(0.,0.,1.));
#9922=DIRECTION('ref_axis',(-1.,0.,0.));
#9923=DIRECTION('',(0.,0.,1.));
#9924=DIRECTION('center_axis',(0.,0.,1.));
#9925=DIRECTION('ref_axis',(-1.,0.,0.));
#9926=DIRECTION('',(0.,0.,1.));
#9927=DIRECTION('center_axis',(0.,0.,1.));
#9928=DIRECTION('ref_axis',(-1.,0.,0.));
#9929=DIRECTION('',(0.,0.,1.));
#9930=DIRECTION('center_axis',(0.,0.,1.));
#9931=DIRECTION('ref_axis',(-1.,0.,0.));
#9932=DIRECTION('',(0.,0.,1.));
#9933=DIRECTION('center_axis',(0.,0.,1.));
#9934=DIRECTION('ref_axis',(-0.937990854518778,-0.346660001787244,0.));
#9935=DIRECTION('',(0.,0.,1.));
#9936=DIRECTION('center_axis',(0.,0.,-1.));
#9937=DIRECTION('ref_axis',(-1.,0.,0.));
#9938=DIRECTION('center_axis',(0.,0.,1.));
#9939=DIRECTION('ref_axis',(-1.,-9.53632271029895E-14,0.));
#9940=DIRECTION('',(-1.22464679914735E-16,-1.16936246806304E-29,1.));
#9941=DIRECTION('center_axis',(0.,0.,-1.));
#9942=DIRECTION('ref_axis',(-1.,-9.53632271029895E-14,0.));
#9943=DIRECTION('center_axis',(0.,0.,1.));
#9944=DIRECTION('ref_axis',(-1.,-9.53632271029895E-14,0.));
#9945=DIRECTION('',(-1.22464679914735E-16,-1.16936246806304E-29,1.));
#9946=DIRECTION('center_axis',(0.,0.,1.));
#9947=DIRECTION('ref_axis',(-1.,-9.53632271029895E-14,0.));
#9948=DIRECTION('',(-1.22464679914735E-16,-1.16936246806304E-29,1.));
#9949=DIRECTION('center_axis',(0.,0.,1.));
#9950=DIRECTION('ref_axis',(-1.,-9.53632271029895E-14,0.));
#9951=DIRECTION('',(-1.22464679914735E-16,-1.16936246806304E-29,1.));
#9952=DIRECTION('center_axis',(0.,0.,1.));
#9953=DIRECTION('ref_axis',(-1.,-9.53632271029895E-14,0.));
#9954=DIRECTION('',(-1.22464679914735E-16,-1.16936246806304E-29,1.));
#9955=DIRECTION('center_axis',(0.,0.,1.));
#9956=DIRECTION('ref_axis',(-1.,-9.53632271029895E-14,0.));
#9957=DIRECTION('',(-1.22464679914735E-16,-1.16936246806304E-29,1.));
#9958=DIRECTION('center_axis',(0.,0.,1.));
#9959=DIRECTION('ref_axis',(-1.,-9.53632271029895E-14,0.));
#9960=DIRECTION('',(-1.22464679914735E-16,-1.16936246806304E-29,1.));
#9961=DIRECTION('center_axis',(0.,0.,1.));
#9962=DIRECTION('ref_axis',(-1.,-9.53632271029895E-14,0.));
#9963=DIRECTION('',(-1.22464679914735E-16,-1.16936246806304E-29,1.));
#9964=DIRECTION('center_axis',(0.,0.,1.));
#9965=DIRECTION('ref_axis',(-1.,-9.53632271029895E-14,0.));
#9966=DIRECTION('',(-1.22464679914735E-16,-1.16936246806304E-29,1.));
#9967=DIRECTION('center_axis',(0.,0.,1.));
#9968=DIRECTION('ref_axis',(-1.,-9.53632271029895E-14,0.));
#9969=DIRECTION('',(-1.22464679914735E-16,-1.16936246806304E-29,1.));
#9970=DIRECTION('center_axis',(0.,0.,1.));
#9971=DIRECTION('ref_axis',(-1.,-9.53632271029895E-14,0.));
#9972=DIRECTION('',(-1.22464679914735E-16,-1.16936246806304E-29,1.));
#9973=DIRECTION('center_axis',(0.,0.,1.));
#9974=DIRECTION('ref_axis',(-1.,-9.53632271029895E-14,0.));
#9975=DIRECTION('',(-1.22464679914735E-16,-1.16936246806304E-29,1.));
#9976=DIRECTION('center_axis',(0.,0.,1.));
#9977=DIRECTION('ref_axis',(-1.,-9.53632271029895E-14,0.));
#9978=DIRECTION('',(-1.22464679914735E-16,-1.16936246806304E-29,1.));
#9979=DIRECTION('center_axis',(0.,0.,1.));
#9980=DIRECTION('ref_axis',(-1.,-9.53632271029895E-14,0.));
#9981=DIRECTION('',(-1.22464679914735E-16,-1.16936246806304E-29,1.));
#9982=DIRECTION('center_axis',(0.,0.,1.));
#9983=DIRECTION('ref_axis',(-1.,-9.53632271029895E-14,0.));
#9984=DIRECTION('',(-1.22464679914735E-16,-1.16936246806304E-29,1.));
#9985=DIRECTION('center_axis',(0.,0.,1.));
#9986=DIRECTION('ref_axis',(-1.,-9.53632271029895E-14,0.));
#9987=DIRECTION('',(-1.22464679914735E-16,-1.16936246806304E-29,1.));
#9988=DIRECTION('center_axis',(0.,0.,1.));
#9989=DIRECTION('ref_axis',(0.609237469603756,-0.792987834478444,0.));
#9990=DIRECTION('',(-1.22464679914735E-16,-1.16936246806304E-29,1.));
#9991=DIRECTION('center_axis',(0.,0.,1.));
#9992=DIRECTION('ref_axis',(-1.,-9.53632271029895E-14,0.));
#9993=DIRECTION('center_axis',(0.,0.,1.));
#9994=DIRECTION('ref_axis',(1.,0.,0.));
#9995=DIRECTION('center_axis',(0.,0.,1.));
#9996=DIRECTION('ref_axis',(-1.,-9.53632271029895E-14,0.));
#9997=DIRECTION('center_axis',(0.,0.,1.));
#9998=DIRECTION('ref_axis',(-1.,0.,0.));
#9999=DIRECTION('center_axis',(0.,0.,1.));
#10000=DIRECTION('ref_axis',(1.,0.,0.));
#10001=DIRECTION('center_axis',(0.,0.,1.));
#10002=DIRECTION('ref_axis',(-1.,-1.01142816624385E-13,0.));
#10003=DIRECTION('center_axis',(0.,0.,1.));
#10004=DIRECTION('ref_axis',(-1.,0.,0.));
#10005=DIRECTION('center_axis',(0.,0.,1.));
#10006=DIRECTION('ref_axis',(1.,0.,0.));
#10007=DIRECTION('center_axis',(0.,0.,1.));
#10008=DIRECTION('ref_axis',(-1.,-1.09812200906474E-13,0.));
#10009=DIRECTION('center_axis',(0.,0.,1.));
#10010=DIRECTION('ref_axis',(-1.,0.,0.));
#10011=DIRECTION('center_axis',(0.,0.,1.));
#10012=DIRECTION('ref_axis',(1.,0.,0.));
#10013=DIRECTION('center_axis',(0.,0.,1.));
#10014=DIRECTION('ref_axis',(-1.,-9.82530218636873E-14,0.));
#10015=DIRECTION('center_axis',(0.,0.,1.));
#10016=DIRECTION('ref_axis',(-1.,0.,0.));
#10017=DIRECTION('center_axis',(0.,0.,1.));
#10018=DIRECTION('ref_axis',(-1.,0.,0.));
#10019=DIRECTION('center_axis',(0.,0.,1.));
#10020=DIRECTION('ref_axis',(-1.,0.,0.));
#10021=DIRECTION('center_axis',(0.,0.,1.));
#10022=DIRECTION('ref_axis',(-1.,0.,0.));
#10023=DIRECTION('center_axis',(0.,0.,1.));
#10024=DIRECTION('ref_axis',(-1.,0.,0.));
#10025=DIRECTION('center_axis',(0.,1.,0.));
#10026=DIRECTION('ref_axis',(-1.,0.,0.));
#10027=DIRECTION('',(-1.,0.,0.));
#10028=DIRECTION('',(0.,0.,1.));
#10029=DIRECTION('',(-1.,0.,0.));
#10030=DIRECTION('',(0.,0.,1.));
#10031=DIRECTION('center_axis',(-1.,0.,0.));
#10032=DIRECTION('ref_axis',(0.,-1.,0.));
#10033=DIRECTION('',(0.,-1.,0.));
#10034=DIRECTION('',(0.,-1.,0.));
#10035=DIRECTION('',(0.,0.,1.));
#10036=DIRECTION('center_axis',(0.,-1.,0.));
#10037=DIRECTION('ref_axis',(1.,0.,0.));
#10038=DIRECTION('',(1.,0.,0.));
#10039=DIRECTION('',(1.,0.,0.));
#10040=DIRECTION('',(0.,0.,1.));
#10041=DIRECTION('center_axis',(1.,0.,0.));
#10042=DIRECTION('ref_axis',(0.,1.,0.));
#10043=DIRECTION('',(0.,1.,0.));
#10044=DIRECTION('',(0.,1.,0.));
#10045=DIRECTION('center_axis',(0.,1.,0.));
#10046=DIRECTION('ref_axis',(-1.,0.,0.));
#10047=DIRECTION('',(1.,0.,0.));
#10048=DIRECTION('',(0.,0.,1.));
#10049=DIRECTION('',(1.,0.,0.));
#10050=DIRECTION('',(0.,0.,-1.));
#10051=DIRECTION('center_axis',(1.,0.,0.));
#10052=DIRECTION('ref_axis',(0.,1.,0.));
#10053=DIRECTION('',(0.,-1.,0.));
#10054=DIRECTION('',(0.,-1.,0.));
#10055=DIRECTION('',(0.,0.,-1.));
#10056=DIRECTION('center_axis',(0.,-1.,0.));
#10057=DIRECTION('ref_axis',(1.,0.,0.));
#10058=DIRECTION('',(-1.,0.,0.));
#10059=DIRECTION('',(-1.,0.,0.));
#10060=DIRECTION('',(0.,0.,1.));
#10061=DIRECTION('center_axis',(-1.,0.,0.));
#10062=DIRECTION('ref_axis',(0.,-1.,0.));
#10063=DIRECTION('',(0.,1.,0.));
#10064=DIRECTION('',(0.,1.,0.));
#10065=DIRECTION('center_axis',(0.,0.,1.));
#10066=DIRECTION('ref_axis',(1.,0.,0.));
#10067=DIRECTION('center_axis',(0.,0.,1.));
#10068=DIRECTION('ref_axis',(1.,0.,0.));
#10069=DIRECTION('axis',(0.,0.,1.));
#10070=DIRECTION('refdir',(1.,0.,0.));
#10071=DIRECTION('center_axis',(0.,0.,-1.));
#10072=DIRECTION('ref_axis',(1.,0.,0.));
#10073=DIRECTION('center_axis',(0.,0.,-1.));
#10074=DIRECTION('ref_axis',(1.,0.,0.));
#10075=DIRECTION('',(0.,0.,-1.));
#10076=DIRECTION('center_axis',(0.,0.,1.));
#10077=DIRECTION('ref_axis',(1.,0.,0.));
#10078=DIRECTION('center_axis',(0.,0.,-1.));
#10079=DIRECTION('ref_axis',(1.,0.,0.));
#10080=DIRECTION('center_axis',(0.,0.,-1.));
#10081=DIRECTION('ref_axis',(1.,0.,0.));
#10082=DIRECTION('',(0.,0.,-1.));
#10083=DIRECTION('center_axis',(0.,0.,1.));
#10084=DIRECTION('ref_axis',(1.,0.,0.));
#10085=DIRECTION('center_axis',(0.,0.,-1.));
#10086=DIRECTION('ref_axis',(1.,0.,0.));
#10087=DIRECTION('center_axis',(0.,0.,-1.));
#10088=DIRECTION('ref_axis',(1.,0.,0.));
#10089=DIRECTION('',(0.,0.,-1.));
#10090=DIRECTION('center_axis',(0.,0.,1.));
#10091=DIRECTION('ref_axis',(1.,0.,0.));
#10092=DIRECTION('center_axis',(0.,0.,-1.));
#10093=DIRECTION('ref_axis',(1.,0.,0.));
#10094=DIRECTION('center_axis',(0.,0.,-1.));
#10095=DIRECTION('ref_axis',(1.,0.,0.));
#10096=DIRECTION('',(0.,0.,-1.));
#10097=DIRECTION('center_axis',(0.,0.,1.));
#10098=DIRECTION('ref_axis',(1.,0.,0.));
#10099=DIRECTION('center_axis',(0.,0.,-1.));
#10100=DIRECTION('ref_axis',(1.,0.,0.));
#10101=DIRECTION('center_axis',(0.,0.,-1.));
#10102=DIRECTION('ref_axis',(1.,0.,0.));
#10103=DIRECTION('',(0.,0.,-1.));
#10104=DIRECTION('center_axis',(0.,0.,1.));
#10105=DIRECTION('ref_axis',(1.,0.,0.));
#10106=DIRECTION('center_axis',(0.,1.,0.));
#10107=DIRECTION('ref_axis',(-1.,0.,0.));
#10108=DIRECTION('',(-1.,0.,0.));
#10109=DIRECTION('',(0.,0.,1.));
#10110=DIRECTION('',(-1.,0.,0.));
#10111=DIRECTION('',(0.,0.,1.));
#10112=DIRECTION('center_axis',(1.,0.,0.));
#10113=DIRECTION('ref_axis',(0.,1.,0.));
#10114=DIRECTION('',(0.,1.,0.));
#10115=DIRECTION('',(0.,1.,0.));
#10116=DIRECTION('',(0.,0.,1.));
#10117=DIRECTION('center_axis',(0.,-1.,0.));
#10118=DIRECTION('ref_axis',(1.,0.,0.));
#10119=DIRECTION('',(1.,0.,0.));
#10120=DIRECTION('',(1.,0.,0.));
#10121=DIRECTION('',(0.,0.,1.));
#10122=DIRECTION('center_axis',(-1.,0.,0.));
#10123=DIRECTION('ref_axis',(0.,-1.,0.));
#10124=DIRECTION('',(0.,-1.,0.));
#10125=DIRECTION('',(0.,-1.,0.));
#10126=DIRECTION('center_axis',(0.,0.,1.));
#10127=DIRECTION('ref_axis',(1.,0.,0.));
#10128=DIRECTION('center_axis',(0.,0.,1.));
#10129=DIRECTION('ref_axis',(1.,0.,0.));
#10130=DIRECTION('axis',(0.,0.,1.));
#10131=DIRECTION('refdir',(1.,0.,0.));
#10132=DIRECTION('center_axis',(0.,1.,0.));
#10133=DIRECTION('ref_axis',(-1.,0.,0.));
#10134=DIRECTION('',(-1.,0.,0.));
#10135=DIRECTION('',(0.,0.,1.));
#10136=DIRECTION('',(-1.,0.,0.));
#10137=DIRECTION('',(0.,0.,1.));
#10138=DIRECTION('center_axis',(-1.,0.,0.));
#10139=DIRECTION('ref_axis',(0.,-1.,0.));
#10140=DIRECTION('',(0.,-1.,0.));
#10141=DIRECTION('',(0.,-1.,0.));
#10142=DIRECTION('',(0.,0.,1.));
#10143=DIRECTION('center_axis',(0.,-1.,0.));
#10144=DIRECTION('ref_axis',(1.,0.,0.));
#10145=DIRECTION('',(1.,0.,0.));
#10146=DIRECTION('',(1.,0.,0.));
#10147=DIRECTION('',(0.,0.,1.));
#10148=DIRECTION('center_axis',(1.,0.,0.));
#10149=DIRECTION('ref_axis',(0.,1.,0.));
#10150=DIRECTION('',(0.,1.,0.));
#10151=DIRECTION('',(0.,1.,0.));
#10152=DIRECTION('center_axis',(0.,1.,0.));
#10153=DIRECTION('ref_axis',(-1.,0.,0.));
#10154=DIRECTION('',(-1.,0.,0.));
#10155=DIRECTION('',(0.,0.,1.));
#10156=DIRECTION('',(-1.,0.,0.));
#10157=DIRECTION('',(0.,0.,1.));
#10158=DIRECTION('center_axis',(1.,0.,0.));
#10159=DIRECTION('ref_axis',(0.,1.,0.));
#10160=DIRECTION('',(0.,1.,0.));
#10161=DIRECTION('',(0.,1.,0.));
#10162=DIRECTION('',(0.,0.,1.));
#10163=DIRECTION('center_axis',(0.,-1.,0.));
#10164=DIRECTION('ref_axis',(1.,0.,0.));
#10165=DIRECTION('',(1.,0.,0.));
#10166=DIRECTION('',(1.,0.,0.));
#10167=DIRECTION('',(0.,0.,1.));
#10168=DIRECTION('center_axis',(-1.,0.,0.));
#10169=DIRECTION('ref_axis',(0.,-1.,0.));
#10170=DIRECTION('',(0.,-1.,0.));
#10171=DIRECTION('',(0.,-1.,0.));
#10172=DIRECTION('center_axis',(0.,0.,1.));
#10173=DIRECTION('ref_axis',(1.,0.,0.));
#10174=DIRECTION('center_axis',(0.,0.,1.));
#10175=DIRECTION('ref_axis',(1.,0.,0.));
#10176=DIRECTION('axis',(0.,0.,1.));
#10177=DIRECTION('refdir',(1.,0.,0.));
#10178=DIRECTION('center_axis',(0.,0.,-1.));
#10179=DIRECTION('ref_axis',(1.,0.,0.));
#10180=DIRECTION('',(0.,0.,-1.));
#10181=DIRECTION('center_axis',(0.,0.,1.));
#10182=DIRECTION('ref_axis',(1.,0.,0.));
#10183=DIRECTION('',(0.,0.,-1.));
#10184=DIRECTION('center_axis',(0.,0.,1.));
#10185=DIRECTION('ref_axis',(1.,0.,0.));
#10186=DIRECTION('center_axis',(0.,0.,-1.));
#10187=DIRECTION('ref_axis',(1.,0.,0.));
#10188=DIRECTION('',(0.,0.,-1.));
#10189=DIRECTION('center_axis',(0.,0.,-1.));
#10190=DIRECTION('ref_axis',(1.,0.,0.));
#10191=DIRECTION('',(0.,0.,-1.));
#10192=DIRECTION('center_axis',(0.,0.,-1.));
#10193=DIRECTION('ref_axis',(1.,0.,0.));
#10194=DIRECTION('',(0.,0.,-1.));
#10195=DIRECTION('center_axis',(0.,0.,-1.));
#10196=DIRECTION('ref_axis',(1.,0.,0.));
#10197=DIRECTION('',(0.,0.,-1.));
#10198=DIRECTION('center_axis',(0.,0.,-1.));
#10199=DIRECTION('ref_axis',(1.,0.,0.));
#10200=DIRECTION('',(0.,0.,-1.));
#10201=DIRECTION('center_axis',(0.,0.,-1.));
#10202=DIRECTION('ref_axis',(1.,0.,0.));
#10203=DIRECTION('',(0.,0.,-1.));
#10204=DIRECTION('center_axis',(0.,0.,-1.));
#10205=DIRECTION('ref_axis',(1.,0.,0.));
#10206=DIRECTION('',(0.,0.,-1.));
#10207=DIRECTION('center_axis',(0.,0.,-1.));
#10208=DIRECTION('ref_axis',(1.,0.,0.));
#10209=DIRECTION('',(0.,0.,-1.));
#10210=DIRECTION('center_axis',(0.,0.,-1.));
#10211=DIRECTION('ref_axis',(1.,0.,0.));
#10212=DIRECTION('',(0.,0.,-1.));
#10213=DIRECTION('center_axis',(0.,0.,-1.));
#10214=DIRECTION('ref_axis',(1.,0.,0.));
#10215=DIRECTION('',(0.,0.,-1.));
#10216=DIRECTION('center_axis',(0.,0.,-1.));
#10217=DIRECTION('ref_axis',(1.,0.,0.));
#10218=DIRECTION('',(0.,0.,-1.));
#10219=DIRECTION('center_axis',(0.,0.,-1.));
#10220=DIRECTION('ref_axis',(1.,0.,0.));
#10221=DIRECTION('',(0.,0.,-1.));
#10222=DIRECTION('center_axis',(0.,0.,-1.));
#10223=DIRECTION('ref_axis',(1.,0.,0.));
#10224=DIRECTION('',(0.,0.,-1.));
#10225=DIRECTION('center_axis',(0.,0.,-1.));
#10226=DIRECTION('ref_axis',(0.938434895654951,-0.34545614282725,0.));
#10227=DIRECTION('',(0.,0.,-1.));
#10228=DIRECTION('center_axis',(0.,0.,-1.));
#10229=DIRECTION('ref_axis',(1.,0.,0.));
#10230=DIRECTION('center_axis',(0.,0.,-1.));
#10231=DIRECTION('ref_axis',(0.0179472551277058,0.999838935045731,0.));
#10232=DIRECTION('',(1.22464679914735E-16,-9.43079471310298E-30,-1.));
#10233=DIRECTION('center_axis',(0.,0.,1.));
#10234=DIRECTION('ref_axis',(1.,-7.68858181953524E-14,0.));
#10235=DIRECTION('center_axis',(0.,0.,-1.));
#10236=DIRECTION('ref_axis',(1.,-7.68858181953524E-14,0.));
#10237=DIRECTION('',(1.22464679914735E-16,-9.43079471310298E-30,-1.));
#10238=DIRECTION('center_axis',(0.,0.,-1.));
#10239=DIRECTION('ref_axis',(1.,-7.68858181953524E-14,0.));
#10240=DIRECTION('',(1.22464679914735E-16,-9.43079471310298E-30,-1.));
#10241=DIRECTION('center_axis',(0.,0.,-1.));
#10242=DIRECTION('ref_axis',(1.,-7.68858181953524E-14,0.));
#10243=DIRECTION('',(1.22464679914735E-16,-9.43079471310298E-30,-1.));
#10244=DIRECTION('center_axis',(0.,0.,-1.));
#10245=DIRECTION('ref_axis',(1.,-7.68858181953524E-14,0.));
#10246=DIRECTION('',(1.22464679914735E-16,-9.43079471310298E-30,-1.));
#10247=DIRECTION('center_axis',(0.,0.,-1.));
#10248=DIRECTION('ref_axis',(1.,-7.68858181953524E-14,0.));
#10249=DIRECTION('',(1.22464679914735E-16,-9.43079471310298E-30,-1.));
#10250=DIRECTION('center_axis',(0.,0.,-1.));
#10251=DIRECTION('ref_axis',(1.,-7.68858181953524E-14,0.));
#10252=DIRECTION('',(1.22464679914735E-16,-9.43079471310298E-30,-1.));
#10253=DIRECTION('center_axis',(0.,0.,-1.));
#10254=DIRECTION('ref_axis',(1.,-7.68858181953524E-14,0.));
#10255=DIRECTION('',(1.22464679914735E-16,-9.43079471310298E-30,-1.));
#10256=DIRECTION('center_axis',(0.,0.,-1.));
#10257=DIRECTION('ref_axis',(1.,-7.68858181953524E-14,0.));
#10258=DIRECTION('',(1.22464679914735E-16,-9.43079471310298E-30,-1.));
#10259=DIRECTION('center_axis',(0.,0.,-1.));
#10260=DIRECTION('ref_axis',(1.,-7.68858181953524E-14,0.));
#10261=DIRECTION('',(1.22464679914735E-16,-9.43079471310298E-30,-1.));
#10262=DIRECTION('center_axis',(0.,0.,-1.));
#10263=DIRECTION('ref_axis',(1.,-7.68858181953524E-14,0.));
#10264=DIRECTION('',(1.22464679914735E-16,-9.43079471310298E-30,-1.));
#10265=DIRECTION('center_axis',(0.,0.,-1.));
#10266=DIRECTION('ref_axis',(1.,-7.68858181953524E-14,0.));
#10267=DIRECTION('',(1.22464679914735E-16,-9.43079471310298E-30,-1.));
#10268=DIRECTION('center_axis',(0.,0.,-1.));
#10269=DIRECTION('ref_axis',(1.,-7.68858181953524E-14,0.));
#10270=DIRECTION('',(1.22464679914735E-16,-9.43079471310298E-30,-1.));
#10271=DIRECTION('center_axis',(0.,0.,-1.));
#10272=DIRECTION('ref_axis',(1.,-7.68858181953524E-14,0.));
#10273=DIRECTION('',(1.22464679914735E-16,-9.43079471310298E-30,-1.));
#10274=DIRECTION('center_axis',(0.,0.,-1.));
#10275=DIRECTION('ref_axis',(1.,-7.68858181953524E-14,0.));
#10276=DIRECTION('',(1.22464679914735E-16,-9.43079471310298E-30,-1.));
#10277=DIRECTION('center_axis',(0.,0.,-1.));
#10278=DIRECTION('ref_axis',(-0.609350010373174,-0.792901358844978,0.));
#10279=DIRECTION('',(1.22464679914735E-16,-9.43079471310298E-30,-1.));
#10280=DIRECTION('center_axis',(0.,0.,-1.));
#10281=DIRECTION('ref_axis',(1.,-7.68858181953524E-14,0.));
#10282=DIRECTION('center_axis',(0.,0.,1.));
#10283=DIRECTION('ref_axis',(1.,0.,0.));
#10284=DIRECTION('center_axis',(0.,0.,-1.));
#10285=DIRECTION('ref_axis',(1.,-7.68858181953524E-14,0.));
#10286=DIRECTION('center_axis',(0.,0.,-1.));
#10287=DIRECTION('ref_axis',(1.,0.,0.));
#10288=DIRECTION('center_axis',(0.,0.,-1.));
#10289=DIRECTION('ref_axis',(1.,0.,0.));
#10290=DIRECTION('center_axis',(0.,-1.,0.));
#10291=DIRECTION('ref_axis',(-1.,0.,0.));
#10292=DIRECTION('',(1.,0.,0.));
#10293=DIRECTION('',(0.,0.,-1.));
#10294=DIRECTION('',(1.,0.,0.));
#10295=DIRECTION('',(0.,0.,-1.));
#10296=DIRECTION('center_axis',(1.,0.,0.));
#10297=DIRECTION('ref_axis',(0.,-1.,0.));
#10298=DIRECTION('',(0.,1.,0.));
#10299=DIRECTION('',(0.,0.,-1.));
#10300=DIRECTION('',(0.,1.,0.));
#10301=DIRECTION('center_axis',(0.,1.,0.));
#10302=DIRECTION('ref_axis',(1.,0.,0.));
#10303=DIRECTION('',(-1.,0.,0.));
#10304=DIRECTION('',(0.,0.,-1.));
#10305=DIRECTION('',(-1.,0.,0.));
#10306=DIRECTION('center_axis',(-1.,0.,0.));
#10307=DIRECTION('ref_axis',(0.,1.,0.));
#10308=DIRECTION('',(0.,-1.,0.));
#10309=DIRECTION('',(0.,-1.,0.));
#10310=DIRECTION('center_axis',(0.,0.,1.));
#10311=DIRECTION('ref_axis',(1.,0.,0.));
#10312=DIRECTION('center_axis',(0.,0.,1.));
#10313=DIRECTION('ref_axis',(1.,0.,0.));
#10314=DIRECTION('center_axis',(0.,0.,1.));
#10315=DIRECTION('ref_axis',(1.,0.,0.));
#10316=DIRECTION('',(0.,0.,1.));
#10317=DIRECTION('center_axis',(0.,0.,1.));
#10318=DIRECTION('ref_axis',(1.,0.,0.));
#10319=DIRECTION('center_axis',(0.,0.,-1.));
#10320=DIRECTION('ref_axis',(-1.,0.,0.));
#10321=DIRECTION('center_axis',(0.,0.,-1.));
#10322=DIRECTION('ref_axis',(1.,0.,0.));
#10323=DIRECTION('center_axis',(0.,0.,1.));
#10324=DIRECTION('ref_axis',(1.,0.,0.));
#10325=DIRECTION('center_axis',(0.,0.,1.));
#10326=DIRECTION('ref_axis',(1.,0.,0.));
#10327=DIRECTION('center_axis',(0.,0.,1.));
#10328=DIRECTION('ref_axis',(1.,0.,0.));
#10329=DIRECTION('center_axis',(0.,0.,1.));
#10330=DIRECTION('ref_axis',(1.,0.,0.));
#10331=DIRECTION('',(0.,0.,-1.));
#10332=DIRECTION('center_axis',(-1.60246890531964E-16,-1.,0.));
#10333=DIRECTION('ref_axis',(1.,-1.60246890531964E-16,0.));
#10334=DIRECTION('',(-1.,1.60246890531964E-16,0.));
#10335=DIRECTION('',(0.,0.,1.));
#10336=DIRECTION('',(1.,-1.60246890531964E-16,0.));
#10337=DIRECTION('',(0.,0.,1.));
#10338=DIRECTION('center_axis',(-0.866025403784439,-0.5,0.));
#10339=DIRECTION('ref_axis',(0.5,-0.866025403784439,0.));
#10340=DIRECTION('',(-0.5,0.866025403784439,0.));
#10341=DIRECTION('',(0.5,-0.866025403784439,0.));
#10342=DIRECTION('',(0.,0.,1.));
#10343=DIRECTION('center_axis',(-0.866025403784439,0.5,0.));
#10344=DIRECTION('ref_axis',(-0.5,-0.866025403784439,0.));
#10345=DIRECTION('',(0.5,0.866025403784439,0.));
#10346=DIRECTION('',(-0.5,-0.866025403784439,0.));
#10347=DIRECTION('',(0.,0.,1.));
#10348=DIRECTION('center_axis',(1.60246890531964E-16,1.,0.));
#10349=DIRECTION('ref_axis',(-1.,1.60246890531964E-16,0.));
#10350=DIRECTION('',(1.,-1.60246890531964E-16,0.));
#10351=DIRECTION('',(-1.,1.60246890531964E-16,0.));
#10352=DIRECTION('',(0.,0.,1.));
#10353=DIRECTION('center_axis',(0.866025403784439,0.5,0.));
#10354=DIRECTION('ref_axis',(-0.5,0.866025403784439,0.));
#10355=DIRECTION('',(0.5,-0.866025403784439,0.));
#10356=DIRECTION('',(-0.5,0.866025403784439,0.));
#10357=DIRECTION('',(0.,0.,1.));
#10358=DIRECTION('center_axis',(0.866025403784439,-0.5,0.));
#10359=DIRECTION('ref_axis',(0.5,0.866025403784439,0.));
#10360=DIRECTION('',(-0.5,-0.866025403784439,0.));
#10361=DIRECTION('',(0.5,0.866025403784439,0.));
#10362=DIRECTION('center_axis',(0.,0.,1.));
#10363=DIRECTION('ref_axis',(1.,0.,0.));
#10364=DIRECTION('center_axis',(0.,0.,1.));
#10365=DIRECTION('ref_axis',(1.,0.,0.));
#10366=DIRECTION('center_axis',(0.,0.,1.));
#10367=DIRECTION('ref_axis',(1.,0.,0.));
#10368=DIRECTION('center_axis',(0.,0.,1.));
#10369=DIRECTION('ref_axis',(1.,0.,0.));
#10370=DIRECTION('center_axis',(0.,0.,1.));
#10371=DIRECTION('ref_axis',(1.,0.,0.));
#10372=DIRECTION('',(0.,0.,-1.));
#10373=DIRECTION('center_axis',(0.,0.,1.));
#10374=DIRECTION('ref_axis',(1.,0.,0.));
#10375=DIRECTION('center_axis',(0.,0.,1.));
#10376=DIRECTION('ref_axis',(1.,0.,0.));
#10377=DIRECTION('center_axis',(0.,0.,1.));
#10378=DIRECTION('ref_axis',(1.,0.,0.));
#10379=DIRECTION('',(0.,0.,-1.));
#10380=DIRECTION('center_axis',(0.,0.,1.));
#10381=DIRECTION('ref_axis',(1.,0.,0.));
#10382=DIRECTION('axis',(0.,0.,1.));
#10383=DIRECTION('refdir',(1.,0.,0.));
#10384=DIRECTION('center_axis',(0.866025403784439,0.5,0.));
#10385=DIRECTION('ref_axis',(0.5,-0.866025403784439,0.));
#10386=DIRECTION('',(0.5,-0.866025403784439,0.));
#10387=DIRECTION('',(0.,0.,-1.));
#10388=DIRECTION('',(-0.5,0.866025403784439,0.));
#10389=DIRECTION('',(0.,0.,-1.));
#10390=DIRECTION('center_axis',(1.60246890531964E-16,1.,0.));
#10391=DIRECTION('ref_axis',(1.,-1.60246890531964E-16,0.));
#10392=DIRECTION('',(1.,-1.60246890531964E-16,0.));
#10393=DIRECTION('',(0.,0.,-1.));
#10394=DIRECTION('',(-1.,1.60246890531964E-16,0.));
#10395=DIRECTION('center_axis',(-0.866025403784439,0.5,0.));
#10396=DIRECTION('ref_axis',(0.5,0.866025403784439,0.));
#10397=DIRECTION('',(0.5,0.866025403784439,0.));
#10398=DIRECTION('',(0.,0.,-1.));
#10399=DIRECTION('',(-0.5,-0.866025403784439,0.));
#10400=DIRECTION('center_axis',(-0.866025403784439,-0.5,0.));
#10401=DIRECTION('ref_axis',(-0.5,0.866025403784439,0.));
#10402=DIRECTION('',(-0.5,0.866025403784439,0.));
#10403=DIRECTION('',(0.,0.,-1.));
#10404=DIRECTION('',(0.5,-0.866025403784439,0.));
#10405=DIRECTION('center_axis',(-1.60246890531964E-16,-1.,0.));
#10406=DIRECTION('ref_axis',(-1.,1.60246890531964E-16,0.));
#10407=DIRECTION('',(-1.,1.60246890531964E-16,0.));
#10408=DIRECTION('',(0.,0.,-1.));
#10409=DIRECTION('',(1.,-1.60246890531964E-16,0.));
#10410=DIRECTION('center_axis',(0.866025403784439,-0.5,0.));
#10411=DIRECTION('ref_axis',(-0.5,-0.866025403784439,0.));
#10412=DIRECTION('',(-0.5,-0.866025403784439,0.));
#10413=DIRECTION('',(0.5,0.866025403784439,0.));
#10414=DIRECTION('center_axis',(0.,1.,0.));
#10415=DIRECTION('ref_axis',(-1.,0.,0.));
#10416=DIRECTION('',(-1.,0.,0.));
#10417=DIRECTION('',(0.,0.,1.));
#10418=DIRECTION('',(-1.,0.,0.));
#10419=DIRECTION('',(0.,0.,1.));
#10420=DIRECTION('center_axis',(1.,0.,0.));
#10421=DIRECTION('ref_axis',(0.,1.,0.));
#10422=DIRECTION('',(0.,1.,0.));
#10423=DIRECTION('',(0.,1.,0.));
#10424=DIRECTION('',(0.,0.,1.));
#10425=DIRECTION('center_axis',(0.,-1.,0.));
#10426=DIRECTION('ref_axis',(1.,0.,0.));
#10427=DIRECTION('',(1.,0.,0.));
#10428=DIRECTION('',(1.,0.,0.));
#10429=DIRECTION('',(0.,0.,1.));
#10430=DIRECTION('center_axis',(-1.,0.,0.));
#10431=DIRECTION('ref_axis',(0.,-1.,0.));
#10432=DIRECTION('',(0.,-1.,0.));
#10433=DIRECTION('',(0.,-1.,0.));
#10434=DIRECTION('center_axis',(0.,0.,1.));
#10435=DIRECTION('ref_axis',(1.,0.,0.));
#10436=DIRECTION('center_axis',(0.,0.,1.));
#10437=DIRECTION('ref_axis',(1.,0.,0.));
#10438=DIRECTION('axis',(0.,0.,1.));
#10439=DIRECTION('refdir',(1.,0.,0.));
#10440=DIRECTION('center_axis',(0.,0.,1.));
#10441=DIRECTION('ref_axis',(1.,0.,0.));
#10442=DIRECTION('center_axis',(0.,0.,-1.));
#10443=DIRECTION('ref_axis',(1.,0.,0.));
#10444=DIRECTION('',(0.,0.,-1.));
#10445=DIRECTION('center_axis',(0.,0.,-1.));
#10446=DIRECTION('ref_axis',(1.,0.,0.));
#10447=DIRECTION('center_axis',(0.,0.,1.));
#10448=DIRECTION('ref_axis',(1.,0.,0.));
#10449=DIRECTION('center_axis',(0.,0.,1.));
#10450=DIRECTION('ref_axis',(1.,0.,0.));
#10451=DIRECTION('',(0.,0.,-1.));
#10452=DIRECTION('center_axis',(0.,0.,1.));
#10453=DIRECTION('ref_axis',(1.,0.,0.));
#10454=DIRECTION('center_axis',(0.,0.,1.));
#10455=DIRECTION('ref_axis',(1.,0.,0.));
#10456=DIRECTION('center_axis',(0.,0.,1.));
#10457=DIRECTION('ref_axis',(1.,0.,0.));
#10458=DIRECTION('axis',(0.,0.,1.));
#10459=DIRECTION('refdir',(1.,0.,0.));
#10460=DIRECTION('center_axis',(-1.,0.,0.));
#10461=DIRECTION('ref_axis',(0.,1.,0.));
#10462=DIRECTION('',(0.,0.,1.));
#10463=DIRECTION('',(0.,-1.,0.));
#10464=DIRECTION('',(0.,0.,-1.));
#10465=DIRECTION('',(0.,1.,0.));
#10466=DIRECTION('center_axis',(1.,0.,0.));
#10467=DIRECTION('ref_axis',(0.,-1.,0.));
#10468=DIRECTION('',(0.,0.,-1.));
#10469=DIRECTION('',(0.,-1.,0.));
#10470=DIRECTION('',(0.,0.,1.));
#10471=DIRECTION('',(0.,1.,0.));
#10472=DIRECTION('center_axis',(0.,0.,1.));
#10473=DIRECTION('ref_axis',(1.,0.,0.));
#10474=DIRECTION('center_axis',(0.,0.,1.));
#10475=DIRECTION('ref_axis',(1.,0.,0.));
#10476=DIRECTION('center_axis',(0.,0.,-1.));
#10477=DIRECTION('ref_axis',(1.,0.,0.));
#10478=DIRECTION('center_axis',(0.,0.,1.));
#10479=DIRECTION('ref_axis',(6.12323399573677E-17,-1.,0.));
#10480=DIRECTION('center_axis',(0.,0.,-1.));
#10481=DIRECTION('ref_axis',(1.,0.,0.));
#10482=DIRECTION('center_axis',(0.,0.,1.));
#10483=DIRECTION('ref_axis',(6.12323399573677E-17,-1.,0.));
#10484=DIRECTION('center_axis',(0.,0.,1.));
#10485=DIRECTION('ref_axis',(1.,0.,0.));
#10486=DIRECTION('center_axis',(0.,0.,1.));
#10487=DIRECTION('ref_axis',(1.,0.,0.));
#10488=DIRECTION('axis',(0.,0.,1.));
#10489=DIRECTION('refdir',(1.,0.,0.));
#10490=DIRECTION('center_axis',(0.,0.,1.));
#10491=DIRECTION('ref_axis',(1.,0.,0.));
#10492=DIRECTION('center_axis',(0.,0.,-1.));
#10493=DIRECTION('ref_axis',(1.,0.,0.));
#10494=DIRECTION('',(0.,0.,-1.));
#10495=DIRECTION('center_axis',(0.,0.,-1.));
#10496=DIRECTION('ref_axis',(1.,0.,0.));
#10497=DIRECTION('center_axis',(0.,0.,1.));
#10498=DIRECTION('ref_axis',(1.,0.,0.));
#10499=DIRECTION('center_axis',(0.,0.,1.));
#10500=DIRECTION('ref_axis',(1.,0.,0.));
#10501=DIRECTION('',(0.,0.,-1.));
#10502=DIRECTION('center_axis',(0.,0.,1.));
#10503=DIRECTION('ref_axis',(1.,0.,0.));
#10504=DIRECTION('center_axis',(0.,0.,1.));
#10505=DIRECTION('ref_axis',(1.,0.,0.));
#10506=DIRECTION('center_axis',(0.,0.,1.));
#10507=DIRECTION('ref_axis',(1.,0.,0.));
#10508=DIRECTION('axis',(0.,0.,1.));
#10509=DIRECTION('refdir',(1.,0.,0.));
#10510=DIRECTION('center_axis',(0.,0.,1.));
#10511=DIRECTION('ref_axis',(1.,0.,0.));
#10512=DIRECTION('',(0.,0.,-1.));
#10513=DIRECTION('center_axis',(0.,0.,-1.));
#10514=DIRECTION('ref_axis',(1.,0.,0.));
#10515=DIRECTION('center_axis',(0.,0.,1.));
#10516=DIRECTION('ref_axis',(1.,0.,0.));
#10517=DIRECTION('',(0.,0.,-1.));
#10518=DIRECTION('center_axis',(0.,0.,1.));
#10519=DIRECTION('ref_axis',(1.,0.,0.));
#10520=DIRECTION('',(0.,0.,-1.));
#10521=DIRECTION('center_axis',(0.,0.,1.));
#10522=DIRECTION('ref_axis',(1.,0.,0.));
#10523=DIRECTION('',(0.,0.,-1.));
#10524=DIRECTION('center_axis',(0.,0.,1.));
#10525=DIRECTION('ref_axis',(1.,0.,0.));
#10526=DIRECTION('',(0.,0.,-1.));
#10527=DIRECTION('center_axis',(0.,0.,1.));
#10528=DIRECTION('ref_axis',(1.,0.,0.));
#10529=DIRECTION('',(0.,0.,-1.));
#10530=DIRECTION('center_axis',(0.,0.,1.));
#10531=DIRECTION('ref_axis',(1.,0.,0.));
#10532=DIRECTION('',(0.,0.,-1.));
#10533=DIRECTION('center_axis',(0.,0.,1.));
#10534=DIRECTION('ref_axis',(1.,0.,0.));
#10535=DIRECTION('',(0.,0.,-1.));
#10536=DIRECTION('center_axis',(0.,0.,1.));
#10537=DIRECTION('ref_axis',(1.,0.,0.));
#10538=DIRECTION('',(0.,0.,-1.));
#10539=DIRECTION('center_axis',(0.,0.,1.));
#10540=DIRECTION('ref_axis',(1.,0.,0.));
#10541=DIRECTION('',(0.,0.,-1.));
#10542=DIRECTION('center_axis',(0.,0.,1.));
#10543=DIRECTION('ref_axis',(0.99867308056793,-0.051498331516286,0.));
#10544=DIRECTION('',(0.,0.,1.));
#10545=DIRECTION('center_axis',(0.,0.,-1.));
#10546=DIRECTION('ref_axis',(1.,5.83250561478606E-14,0.));
#10547=DIRECTION('center_axis',(0.,0.,1.));
#10548=DIRECTION('ref_axis',(1.,5.83250561478606E-14,0.));
#10549=DIRECTION('',(0.,0.,1.));
#10550=DIRECTION('center_axis',(0.,0.,1.));
#10551=DIRECTION('ref_axis',(1.,5.83250561478606E-14,0.));
#10552=DIRECTION('',(0.,0.,1.));
#10553=DIRECTION('center_axis',(0.,0.,1.));
#10554=DIRECTION('ref_axis',(1.,5.83250561478606E-14,0.));
#10555=DIRECTION('',(0.,0.,1.));
#10556=DIRECTION('center_axis',(0.,0.,1.));
#10557=DIRECTION('ref_axis',(1.,5.83250561478606E-14,0.));
#10558=DIRECTION('',(0.,0.,1.));
#10559=DIRECTION('center_axis',(0.,0.,1.));
#10560=DIRECTION('ref_axis',(1.,5.83250561478606E-14,0.));
#10561=DIRECTION('',(0.,0.,1.));
#10562=DIRECTION('center_axis',(0.,0.,1.));
#10563=DIRECTION('ref_axis',(1.,5.83250561478606E-14,0.));
#10564=DIRECTION('',(0.,0.,1.));
#10565=DIRECTION('center_axis',(0.,0.,1.));
#10566=DIRECTION('ref_axis',(1.,5.83250561478606E-14,0.));
#10567=DIRECTION('',(0.,0.,1.));
#10568=DIRECTION('center_axis',(0.,0.,1.));
#10569=DIRECTION('ref_axis',(1.,5.83250561478606E-14,0.));
#10570=DIRECTION('',(0.,0.,1.));
#10571=DIRECTION('center_axis',(0.,0.,1.));
#10572=DIRECTION('ref_axis',(1.,5.83250561478606E-14,0.));
#10573=DIRECTION('',(0.,0.,1.));
#10574=DIRECTION('center_axis',(0.,0.,-1.));
#10575=DIRECTION('ref_axis',(1.,0.,0.));
#10576=DIRECTION('center_axis',(0.,0.,-1.));
#10577=DIRECTION('ref_axis',(1.,0.,0.));
#10578=DIRECTION('',(0.707106781186547,8.65956056235493E-17,0.707106781186548));
#10579=DIRECTION('center_axis',(0.,0.,1.));
#10580=DIRECTION('ref_axis',(1.,0.,0.));
#10581=DIRECTION('center_axis',(0.,0.,1.));
#10582=DIRECTION('ref_axis',(1.,5.83250561478606E-14,0.));
#10583=DIRECTION('center_axis',(0.,0.,-1.));
#10584=DIRECTION('ref_axis',(1.,5.83250561478606E-14,0.));
#10585=DIRECTION('center_axis',(0.,0.,1.));
#10586=DIRECTION('ref_axis',(1.,0.,0.));
#10587=DIRECTION('center_axis',(-1.60246890531964E-16,-1.,0.));
#10588=DIRECTION('ref_axis',(1.,-1.60246890531964E-16,0.));
#10589=DIRECTION('',(1.,-1.60246890531964E-16,0.));
#10590=DIRECTION('',(0.,0.,1.));
#10591=DIRECTION('',(1.,-1.60246890531964E-16,0.));
#10592=DIRECTION('',(0.,0.,1.));
#10593=DIRECTION('center_axis',(-0.866025403784439,-0.5,0.));
#10594=DIRECTION('ref_axis',(0.5,-0.866025403784439,0.));
#10595=DIRECTION('',(0.5,-0.866025403784439,0.));
#10596=DIRECTION('',(0.,0.,1.));
#10597=DIRECTION('',(0.5,-0.866025403784439,0.));
#10598=DIRECTION('center_axis',(-0.866025403784439,0.5,0.));
#10599=DIRECTION('ref_axis',(-0.5,-0.866025403784439,0.));
#10600=DIRECTION('',(-0.5,-0.866025403784439,0.));
#10601=DIRECTION('',(0.,0.,1.));
#10602=DIRECTION('',(-0.5,-0.866025403784439,0.));
#10603=DIRECTION('center_axis',(1.60246890531964E-16,1.,0.));
#10604=DIRECTION('ref_axis',(-1.,1.60246890531964E-16,0.));
#10605=DIRECTION('',(-1.,1.60246890531964E-16,0.));
#10606=DIRECTION('',(0.,0.,1.));
#10607=DIRECTION('',(-1.,1.60246890531964E-16,0.));
#10608=DIRECTION('center_axis',(0.866025403784439,0.5,0.));
#10609=DIRECTION('ref_axis',(-0.5,0.866025403784439,0.));
#10610=DIRECTION('',(-0.5,0.866025403784439,0.));
#10611=DIRECTION('',(0.,0.,1.));
#10612=DIRECTION('',(-0.5,0.866025403784439,0.));
#10613=DIRECTION('center_axis',(0.866025403784439,-0.5,0.));
#10614=DIRECTION('ref_axis',(0.5,0.866025403784439,0.));
#10615=DIRECTION('',(0.5,0.866025403784439,0.));
#10616=DIRECTION('',(0.5,0.866025403784439,0.));
#10617=DIRECTION('center_axis',(0.,0.,1.));
#10618=DIRECTION('ref_axis',(1.,0.,0.));
#10619=DIRECTION('center_axis',(0.,0.,1.));
#10620=DIRECTION('ref_axis',(1.,0.,0.));
#10621=DIRECTION('center_axis',(0.,0.,1.));
#10622=DIRECTION('ref_axis',(1.,0.,0.));
#10623=DIRECTION('center_axis',(0.,0.,1.));
#10624=DIRECTION('ref_axis',(1.,0.,0.));
#10625=DIRECTION('',(0.,0.,-1.));
#10626=DIRECTION('center_axis',(0.,0.,1.));
#10627=DIRECTION('ref_axis',(1.,0.,0.));
#10628=DIRECTION('center_axis',(0.,0.,1.));
#10629=DIRECTION('ref_axis',(1.,0.,0.));
#10630=DIRECTION('center_axis',(0.,0.,1.));
#10631=DIRECTION('ref_axis',(1.,0.,0.));
#10632=DIRECTION('axis',(0.,0.,1.));
#10633=DIRECTION('refdir',(1.,0.,0.));
#10634=DIRECTION('center_axis',(-1.,0.,0.));
#10635=DIRECTION('ref_axis',(0.,1.,0.));
#10636=DIRECTION('',(0.,1.,0.));
#10637=DIRECTION('',(0.,0.,-1.));
#10638=DIRECTION('',(0.,-1.,0.));
#10639=DIRECTION('',(0.,0.,-1.));
#10640=DIRECTION('center_axis',(0.,0.,1.));
#10641=DIRECTION('ref_axis',(1.,0.,0.));
#10642=DIRECTION('',(-1.,0.,0.));
#10643=DIRECTION('',(1.,0.,0.));
#10644=DIRECTION('',(0.,1.,0.));
#10645=DIRECTION('',(-1.,0.,0.));
#10646=DIRECTION('',(0.,-1.,0.));
#10647=DIRECTION('',(1.,0.,0.));
#10648=DIRECTION('',(0.,1.,0.));
#10649=DIRECTION('center_axis',(0.,0.,-1.));
#10650=DIRECTION('ref_axis',(1.,0.,0.));
#10651=DIRECTION('center_axis',(0.,0.,-1.));
#10652=DIRECTION('ref_axis',(1.,0.,0.));
#10653=DIRECTION('center_axis',(0.,0.,-1.));
#10654=DIRECTION('ref_axis',(1.,0.,0.));
#10655=DIRECTION('',(0.,0.,-1.));
#10656=DIRECTION('center_axis',(0.,0.,1.));
#10657=DIRECTION('ref_axis',(1.,0.,0.));
#10658=DIRECTION('center_axis',(0.,0.,-1.));
#10659=DIRECTION('ref_axis',(1.,0.,0.));
#10660=DIRECTION('',(0.,0.,-1.));
#10661=DIRECTION('center_axis',(0.,0.,1.));
#10662=DIRECTION('ref_axis',(1.,0.,0.));
#10663=DIRECTION('center_axis',(0.,1.,0.));
#10664=DIRECTION('ref_axis',(0.547722557505166,0.,-0.836660026534075));
#10665=DIRECTION('',(0.,-1.,0.));
#10666=DIRECTION('center_axis',(0.,1.,0.));
#10667=DIRECTION('ref_axis',(1.,0.,0.));
#10668=DIRECTION('center_axis',(0.,1.,0.));
#10669=DIRECTION('ref_axis',(1.,0.,0.));
#10670=DIRECTION('center_axis',(0.,1.,0.));
#10671=DIRECTION('ref_axis',(1.,0.,0.));
#10672=DIRECTION('center_axis',(0.,-1.,0.));
#10673=DIRECTION('ref_axis',(1.,0.,0.));
#10674=DIRECTION('',(0.,-1.,0.));
#10675=DIRECTION('center_axis',(0.,-1.,0.));
#10676=DIRECTION('ref_axis',(1.,0.,0.));
#10677=DIRECTION('center_axis',(0.,1.,0.));
#10678=DIRECTION('ref_axis',(1.,0.,0.));
#10679=DIRECTION('',(-1.,0.,0.));
#10680=DIRECTION('center_axis',(0.,1.,0.));
#10681=DIRECTION('ref_axis',(1.,0.,0.));
#10682=DIRECTION('',(1.,0.,0.));
#10683=DIRECTION('center_axis',(0.,1.,0.));
#10684=DIRECTION('ref_axis',(1.,0.,0.));
#10685=DIRECTION('center_axis',(0.,-1.,0.));
#10686=DIRECTION('ref_axis',(1.,0.,0.));
#10687=DIRECTION('center_axis',(0.,1.,0.));
#10688=DIRECTION('ref_axis',(1.,0.,0.));
#10689=DIRECTION('',(0.,-1.,0.));
#10690=DIRECTION('center_axis',(0.,-1.,0.));
#10691=DIRECTION('ref_axis',(1.,0.,0.));
#10692=DIRECTION('center_axis',(0.,1.,0.));
#10693=DIRECTION('ref_axis',(0.547722557505166,0.,-0.836660026534075));
#10694=DIRECTION('',(0.,-1.,0.));
#10695=DIRECTION('center_axis',(0.,1.,0.));
#10696=DIRECTION('ref_axis',(1.,0.,0.));
#10697=DIRECTION('center_axis',(0.,-1.,0.));
#10698=DIRECTION('ref_axis',(1.,0.,0.));
#10699=DIRECTION('',(0.,0.,1.));
#10700=DIRECTION('',(1.,0.,0.));
#10701=DIRECTION('center_axis',(0.,1.,0.));
#10702=DIRECTION('ref_axis',(-1.,0.,0.));
#10703=DIRECTION('',(-1.,0.,0.));
#10704=DIRECTION('',(0.,0.,1.));
#10705=DIRECTION('center_axis',(-1.,0.,0.));
#10706=DIRECTION('ref_axis',(0.,-1.,0.));
#10707=DIRECTION('',(0.,-1.,0.));
#10708=DIRECTION('center_axis',(0.,0.,1.));
#10709=DIRECTION('ref_axis',(1.,0.,0.));
#10710=DIRECTION('axis',(0.,0.,1.));
#10711=DIRECTION('refdir',(1.,0.,0.));
#10712=DIRECTION('center_axis',(0.,0.,1.));
#10713=DIRECTION('ref_axis',(1.,0.,0.));
#10714=DIRECTION('center_axis',(0.,0.,1.));
#10715=DIRECTION('ref_axis',(1.,0.,0.));
#10716=DIRECTION('',(0.,0.,1.));
#10717=DIRECTION('center_axis',(0.,0.,1.));
#10718=DIRECTION('ref_axis',(1.,0.,0.));
#10719=DIRECTION('center_axis',(0.,0.,-1.));
#10720=DIRECTION('ref_axis',(-1.,0.,0.));
#10721=DIRECTION('center_axis',(0.,0.,-1.));
#10722=DIRECTION('ref_axis',(1.,0.,0.));
#10723=DIRECTION('center_axis',(0.,0.,1.));
#10724=DIRECTION('ref_axis',(1.,0.,0.));
#10725=DIRECTION('center_axis',(0.,0.,1.));
#10726=DIRECTION('ref_axis',(1.,0.,0.));
#10727=DIRECTION('center_axis',(0.,0.,1.));
#10728=DIRECTION('ref_axis',(1.,0.,0.));
#10729=DIRECTION('center_axis',(0.,0.,1.));
#10730=DIRECTION('ref_axis',(1.,0.,0.));
#10731=DIRECTION('',(0.,0.,-1.));
#10732=DIRECTION('center_axis',(0.,0.,1.));
#10733=DIRECTION('ref_axis',(1.,0.,0.));
#10734=DIRECTION('center_axis',(0.,0.,1.));
#10735=DIRECTION('ref_axis',(1.,0.,0.));
#10736=DIRECTION('center_axis',(0.,0.,1.));
#10737=DIRECTION('ref_axis',(1.,0.,0.));
#10738=DIRECTION('center_axis',(0.,0.,1.));
#10739=DIRECTION('ref_axis',(1.,0.,0.));
#10740=DIRECTION('',(0.,0.,-1.));
#10741=DIRECTION('center_axis',(0.,0.,1.));
#10742=DIRECTION('ref_axis',(1.,0.,0.));
#10743=DIRECTION('center_axis',(0.,0.,1.));
#10744=DIRECTION('ref_axis',(1.,0.,0.));
#10745=DIRECTION('center_axis',(0.,0.,1.));
#10746=DIRECTION('ref_axis',(1.,0.,0.));
#10747=DIRECTION('',(0.,0.,-1.));
#10748=DIRECTION('center_axis',(0.,0.,1.));
#10749=DIRECTION('ref_axis',(1.,0.,0.));
#10750=DIRECTION('axis',(0.,0.,1.));
#10751=DIRECTION('refdir',(1.,0.,0.));
#10752=DIRECTION('center_axis',(-1.,0.,0.));
#10753=DIRECTION('ref_axis',(0.,1.,0.));
#10754=DIRECTION('',(0.,0.,1.));
#10755=DIRECTION('',(0.,-1.,0.));
#10756=DIRECTION('',(0.,0.,-1.));
#10757=DIRECTION('',(0.,1.,0.));
#10758=DIRECTION('center_axis',(1.,0.,0.));
#10759=DIRECTION('ref_axis',(0.,-1.,0.));
#10760=DIRECTION('',(0.,0.,-1.));
#10761=DIRECTION('',(0.,-1.,0.));
#10762=DIRECTION('',(0.,0.,1.));
#10763=DIRECTION('',(0.,1.,0.));
#10764=DIRECTION('center_axis',(0.,0.,1.));
#10765=DIRECTION('ref_axis',(1.,0.,0.));
#10766=DIRECTION('center_axis',(0.,0.,1.));
#10767=DIRECTION('ref_axis',(1.,0.,0.));
#10768=DIRECTION('center_axis',(0.,0.,-1.));
#10769=DIRECTION('ref_axis',(1.,0.,0.));
#10770=DIRECTION('center_axis',(0.,0.,1.));
#10771=DIRECTION('ref_axis',(6.12323399573677E-17,-1.,0.));
#10772=DIRECTION('center_axis',(0.,0.,-1.));
#10773=DIRECTION('ref_axis',(1.,0.,0.));
#10774=DIRECTION('center_axis',(0.,0.,1.));
#10775=DIRECTION('ref_axis',(6.12323399573677E-17,-1.,0.));
#10776=DIRECTION('center_axis',(0.,0.,1.));
#10777=DIRECTION('ref_axis',(1.,0.,0.));
#10778=DIRECTION('center_axis',(0.,0.,1.));
#10779=DIRECTION('ref_axis',(1.,0.,0.));
#10780=DIRECTION('axis',(0.,0.,1.));
#10781=DIRECTION('refdir',(1.,0.,0.));
#10782=DIRECTION('center_axis',(1.,0.,0.));
#10783=DIRECTION('ref_axis',(0.,-1.,0.));
#10784=DIRECTION('',(0.,-1.,0.));
#10785=DIRECTION('',(0.,0.,-1.));
#10786=DIRECTION('',(0.,1.,0.));
#10787=DIRECTION('',(0.,0.,-1.));
#10788=DIRECTION('center_axis',(1.,0.,0.));
#10789=DIRECTION('ref_axis',(0.,-1.,0.));
#10790=DIRECTION('',(0.,-1.,0.));
#10791=DIRECTION('',(0.,0.,1.));
#10792=DIRECTION('',(0.,1.,0.));
#10793=DIRECTION('',(0.,0.,-1.));
#10794=DIRECTION('center_axis',(0.,0.,1.));
#10795=DIRECTION('ref_axis',(1.,0.,0.));
#10796=DIRECTION('',(-1.,0.,0.));
#10797=DIRECTION('',(0.,1.,0.));
#10798=DIRECTION('',(1.,0.,0.));
#10799=DIRECTION('',(-1.,0.,0.));
#10800=DIRECTION('',(0.,1.,0.));
#10801=DIRECTION('',(1.,0.,0.));
#10802=DIRECTION('center_axis',(0.,0.,1.));
#10803=DIRECTION('ref_axis',(1.,0.,0.));
#10804=DIRECTION('center_axis',(0.,0.,1.));
#10805=DIRECTION('ref_axis',(1.,0.,0.));
#10806=DIRECTION('center_axis',(0.,1.,0.));
#10807=DIRECTION('ref_axis',(-1.,0.,0.));
#10808=DIRECTION('',(-1.,0.,0.));
#10809=DIRECTION('',(0.,0.,1.));
#10810=DIRECTION('center_axis',(0.,0.,-1.));
#10811=DIRECTION('ref_axis',(1.,0.,0.));
#10812=DIRECTION('center_axis',(0.,0.,-1.));
#10813=DIRECTION('ref_axis',(1.,0.,0.));
#10814=DIRECTION('',(0.,0.,-1.));
#10815=DIRECTION('center_axis',(0.,0.,-1.));
#10816=DIRECTION('ref_axis',(1.,0.,0.));
#10817=DIRECTION('center_axis',(0.,0.,-1.));
#10818=DIRECTION('ref_axis',(1.,0.,0.));
#10819=DIRECTION('',(0.,0.,-1.));
#10820=DIRECTION('center_axis',(0.,1.,0.));
#10821=DIRECTION('ref_axis',(1.,0.,0.));
#10822=DIRECTION('center_axis',(0.,1.,0.));
#10823=DIRECTION('ref_axis',(1.,0.,0.));
#10824=DIRECTION('',(-1.,0.,0.));
#10825=DIRECTION('center_axis',(0.,-1.,0.));
#10826=DIRECTION('ref_axis',(1.,0.,0.));
#10827=DIRECTION('center_axis',(0.,1.,0.));
#10828=DIRECTION('ref_axis',(1.,0.,0.));
#10829=DIRECTION('',(0.,-1.,0.));
#10830=DIRECTION('center_axis',(0.,-1.,0.));
#10831=DIRECTION('ref_axis',(1.,0.,0.));
#10832=DIRECTION('center_axis',(0.,1.,0.));
#10833=DIRECTION('ref_axis',(-0.547722557505167,0.,-0.836660026534075));
#10834=DIRECTION('',(0.,-1.,0.));
#10835=DIRECTION('center_axis',(0.,1.,0.));
#10836=DIRECTION('ref_axis',(1.,0.,0.));
#10837=DIRECTION('center_axis',(0.,1.,0.));
#10838=DIRECTION('ref_axis',(1.,0.,0.));
#10839=DIRECTION('',(1.,0.,0.));
#10840=DIRECTION('center_axis',(1.,0.,0.));
#10841=DIRECTION('ref_axis',(0.,1.,0.));
#10842=DIRECTION('',(0.,1.,0.));
#10843=DIRECTION('',(0.,0.,1.));
#10844=DIRECTION('center_axis',(0.,-1.,0.));
#10845=DIRECTION('ref_axis',(1.,0.,0.));
#10846=DIRECTION('',(1.,0.,0.));
#10847=DIRECTION('center_axis',(0.,0.,1.));
#10848=DIRECTION('ref_axis',(1.,0.,0.));
#10849=DIRECTION('axis',(0.,0.,1.));
#10850=DIRECTION('refdir',(1.,0.,0.));
#10851=DIRECTION('center_axis',(0.,0.,1.));
#10852=DIRECTION('ref_axis',(1.,0.,0.));
#10853=DIRECTION('center_axis',(0.,0.,-1.));
#10854=DIRECTION('ref_axis',(1.,0.,0.));
#10855=DIRECTION('',(0.,0.,-1.));
#10856=DIRECTION('center_axis',(0.,0.,-1.));
#10857=DIRECTION('ref_axis',(1.,0.,0.));
#10858=DIRECTION('center_axis',(0.,0.,1.));
#10859=DIRECTION('ref_axis',(1.,0.,0.));
#10860=DIRECTION('center_axis',(0.,0.,1.));
#10861=DIRECTION('ref_axis',(1.,0.,0.));
#10862=DIRECTION('',(0.,0.,-1.));
#10863=DIRECTION('center_axis',(0.,0.,1.));
#10864=DIRECTION('ref_axis',(1.,0.,0.));
#10865=DIRECTION('center_axis',(0.,0.,1.));
#10866=DIRECTION('ref_axis',(1.,0.,0.));
#10867=DIRECTION('center_axis',(0.,0.,1.));
#10868=DIRECTION('ref_axis',(1.,0.,0.));
#10869=DIRECTION('axis',(0.,0.,1.));
#10870=DIRECTION('refdir',(1.,0.,0.));
#10871=DIRECTION('center_axis',(0.,0.,1.));
#10872=DIRECTION('ref_axis',(1.,0.,0.));
#10873=DIRECTION('',(0.,0.,-1.));
#10874=DIRECTION('center_axis',(0.,0.,-1.));
#10875=DIRECTION('ref_axis',(1.,0.,0.));
#10876=DIRECTION('center_axis',(0.,0.,1.));
#10877=DIRECTION('ref_axis',(1.,0.,0.));
#10878=DIRECTION('',(0.,0.,-1.));
#10879=DIRECTION('center_axis',(0.,0.,1.));
#10880=DIRECTION('ref_axis',(1.,0.,0.));
#10881=DIRECTION('',(0.,0.,-1.));
#10882=DIRECTION('center_axis',(0.,0.,1.));
#10883=DIRECTION('ref_axis',(1.,0.,0.));
#10884=DIRECTION('',(0.,0.,-1.));
#10885=DIRECTION('center_axis',(0.,0.,1.));
#10886=DIRECTION('ref_axis',(1.,0.,0.));
#10887=DIRECTION('',(0.,0.,-1.));
#10888=DIRECTION('center_axis',(0.,0.,1.));
#10889=DIRECTION('ref_axis',(1.,0.,0.));
#10890=DIRECTION('',(0.,0.,-1.));
#10891=DIRECTION('center_axis',(0.,0.,1.));
#10892=DIRECTION('ref_axis',(1.,0.,0.));
#10893=DIRECTION('',(0.,0.,-1.));
#10894=DIRECTION('center_axis',(0.,0.,1.));
#10895=DIRECTION('ref_axis',(1.,0.,0.));
#10896=DIRECTION('',(0.,0.,-1.));
#10897=DIRECTION('center_axis',(0.,0.,1.));
#10898=DIRECTION('ref_axis',(1.,0.,0.));
#10899=DIRECTION('',(0.,0.,-1.));
#10900=DIRECTION('center_axis',(0.,0.,1.));
#10901=DIRECTION('ref_axis',(1.,0.,0.));
#10902=DIRECTION('',(0.,0.,-1.));
#10903=DIRECTION('center_axis',(0.,0.,1.));
#10904=DIRECTION('ref_axis',(1.,0.,0.));
#10905=DIRECTION('',(0.,0.,-1.));
#10906=DIRECTION('center_axis',(0.,0.,1.));
#10907=DIRECTION('ref_axis',(1.,0.,0.));
#10908=DIRECTION('',(0.,0.,-1.));
#10909=DIRECTION('center_axis',(0.,0.,1.));
#10910=DIRECTION('ref_axis',(1.,0.,0.));
#10911=DIRECTION('',(0.,0.,-1.));
#10912=DIRECTION('center_axis',(0.,0.,1.));
#10913=DIRECTION('ref_axis',(1.,0.,0.));
#10914=DIRECTION('',(0.,0.,-1.));
#10915=DIRECTION('center_axis',(0.,0.,1.));
#10916=DIRECTION('ref_axis',(1.,0.,0.));
#10917=DIRECTION('',(0.,0.,-1.));
#10918=DIRECTION('center_axis',(0.,0.,1.));
#10919=DIRECTION('ref_axis',(1.,0.,0.));
#10920=DIRECTION('',(0.,0.,-1.));
#10921=DIRECTION('center_axis',(0.,0.,1.));
#10922=DIRECTION('ref_axis',(1.,0.,0.));
#10923=DIRECTION('',(0.,0.,-1.));
#10924=DIRECTION('center_axis',(0.,0.,1.));
#10925=DIRECTION('ref_axis',(1.,0.,0.));
#10926=DIRECTION('',(0.,0.,-1.));
#10927=DIRECTION('center_axis',(0.,0.,1.));
#10928=DIRECTION('ref_axis',(1.,0.,0.));
#10929=DIRECTION('',(0.,0.,-1.));
#10930=DIRECTION('center_axis',(0.,0.,1.));
#10931=DIRECTION('ref_axis',(0.997337382943289,-0.0729256099311623,0.));
#10932=DIRECTION('',(0.,0.,1.));
#10933=DIRECTION('center_axis',(0.,0.,-1.));
#10934=DIRECTION('ref_axis',(1.,7.52212518638754E-14,0.));
#10935=DIRECTION('center_axis',(0.,0.,1.));
#10936=DIRECTION('ref_axis',(1.,7.52212518638754E-14,0.));
#10937=DIRECTION('',(0.,0.,1.));
#10938=DIRECTION('center_axis',(0.,0.,1.));
#10939=DIRECTION('ref_axis',(1.,7.52212518638754E-14,0.));
#10940=DIRECTION('',(0.,0.,1.));
#10941=DIRECTION('center_axis',(0.,0.,1.));
#10942=DIRECTION('ref_axis',(1.,7.52212518638754E-14,0.));
#10943=DIRECTION('',(0.,0.,1.));
#10944=DIRECTION('center_axis',(0.,0.,1.));
#10945=DIRECTION('ref_axis',(1.,7.52212518638754E-14,0.));
#10946=DIRECTION('',(0.,0.,1.));
#10947=DIRECTION('center_axis',(0.,0.,1.));
#10948=DIRECTION('ref_axis',(1.,7.52212518638754E-14,0.));
#10949=DIRECTION('',(0.,0.,1.));
#10950=DIRECTION('center_axis',(0.,0.,1.));
#10951=DIRECTION('ref_axis',(1.,7.52212518638754E-14,0.));
#10952=DIRECTION('',(0.,0.,1.));
#10953=DIRECTION('center_axis',(0.,0.,1.));
#10954=DIRECTION('ref_axis',(1.,7.52212518638754E-14,0.));
#10955=DIRECTION('',(0.,0.,1.));
#10956=DIRECTION('center_axis',(0.,0.,1.));
#10957=DIRECTION('ref_axis',(1.,7.52212518638754E-14,0.));
#10958=DIRECTION('',(0.,0.,1.));
#10959=DIRECTION('center_axis',(0.,0.,1.));
#10960=DIRECTION('ref_axis',(1.,7.52212518638754E-14,0.));
#10961=DIRECTION('',(0.,0.,1.));
#10962=DIRECTION('center_axis',(0.,0.,1.));
#10963=DIRECTION('ref_axis',(1.,7.52212518638754E-14,0.));
#10964=DIRECTION('',(0.,0.,1.));
#10965=DIRECTION('center_axis',(0.,0.,1.));
#10966=DIRECTION('ref_axis',(1.,7.52212518638754E-14,0.));
#10967=DIRECTION('',(0.,0.,1.));
#10968=DIRECTION('center_axis',(0.,0.,1.));
#10969=DIRECTION('ref_axis',(1.,7.52212518638754E-14,0.));
#10970=DIRECTION('',(0.,0.,1.));
#10971=DIRECTION('center_axis',(0.,0.,1.));
#10972=DIRECTION('ref_axis',(1.,7.52212518638754E-14,0.));
#10973=DIRECTION('',(0.,0.,1.));
#10974=DIRECTION('center_axis',(0.,0.,1.));
#10975=DIRECTION('ref_axis',(1.,7.52212518638754E-14,0.));
#10976=DIRECTION('',(0.,0.,1.));
#10977=DIRECTION('center_axis',(0.,0.,1.));
#10978=DIRECTION('ref_axis',(1.,7.52212518638754E-14,0.));
#10979=DIRECTION('',(0.,0.,1.));
#10980=DIRECTION('center_axis',(0.,0.,1.));
#10981=DIRECTION('ref_axis',(1.,7.52212518638754E-14,0.));
#10982=DIRECTION('',(0.,0.,1.));
#10983=DIRECTION('center_axis',(0.,0.,1.));
#10984=DIRECTION('ref_axis',(1.,7.52212518638754E-14,0.));
#10985=DIRECTION('',(0.,0.,1.));
#10986=DIRECTION('center_axis',(0.,0.,1.));
#10987=DIRECTION('ref_axis',(1.,7.52212518638754E-14,0.));
#10988=DIRECTION('',(0.,0.,1.));
#10989=DIRECTION('center_axis',(0.,0.,-1.));
#10990=DIRECTION('ref_axis',(1.,0.,0.));
#10991=DIRECTION('center_axis',(0.,0.,-1.));
#10992=DIRECTION('ref_axis',(1.,0.,0.));
#10993=DIRECTION('',(0.707106781186547,8.65956056235493E-17,0.707106781186548));
#10994=DIRECTION('center_axis',(0.,0.,1.));
#10995=DIRECTION('ref_axis',(1.,0.,0.));
#10996=DIRECTION('center_axis',(0.,0.,1.));
#10997=DIRECTION('ref_axis',(1.,7.52212518638754E-14,0.));
#10998=DIRECTION('center_axis',(0.,0.,-1.));
#10999=DIRECTION('ref_axis',(1.,7.52212518638754E-14,0.));
#11000=DIRECTION('center_axis',(0.,0.,1.));
#11001=DIRECTION('ref_axis',(1.,0.,0.));
#11002=DIRECTION('center_axis',(-1.92296268638356E-16,-1.,0.));
#11003=DIRECTION('ref_axis',(1.,-1.92296268638356E-16,0.));
#11004=DIRECTION('',(1.,-1.92296268638356E-16,0.));
#11005=DIRECTION('',(0.,0.,1.));
#11006=DIRECTION('',(1.,-1.92296268638356E-16,0.));
#11007=DIRECTION('',(0.,0.,1.));
#11008=DIRECTION('center_axis',(-0.866025403784439,-0.5,0.));
#11009=DIRECTION('ref_axis',(0.5,-0.866025403784439,0.));
#11010=DIRECTION('',(0.5,-0.866025403784439,0.));
#11011=DIRECTION('',(0.,0.,1.));
#11012=DIRECTION('',(0.5,-0.866025403784439,0.));
#11013=DIRECTION('center_axis',(-0.866025403784439,0.5,0.));
#11014=DIRECTION('ref_axis',(-0.5,-0.866025403784438,0.));
#11015=DIRECTION('',(-0.5,-0.866025403784438,0.));
#11016=DIRECTION('',(0.,0.,1.));
#11017=DIRECTION('',(-0.5,-0.866025403784439,0.));
#11018=DIRECTION('center_axis',(1.92296268638356E-16,1.,0.));
#11019=DIRECTION('ref_axis',(-1.,1.92296268638356E-16,0.));
#11020=DIRECTION('',(-1.,1.92296268638356E-16,0.));
#11021=DIRECTION('',(0.,0.,1.));
#11022=DIRECTION('',(-1.,1.92296268638356E-16,0.));
#11023=DIRECTION('center_axis',(0.866025403784439,0.5,0.));
#11024=DIRECTION('ref_axis',(-0.5,0.866025403784439,0.));
#11025=DIRECTION('',(-0.5,0.866025403784439,0.));
#11026=DIRECTION('',(0.,0.,1.));
#11027=DIRECTION('',(-0.5,0.866025403784439,0.));
#11028=DIRECTION('center_axis',(0.866025403784439,-0.5,0.));
#11029=DIRECTION('ref_axis',(0.5,0.866025403784439,0.));
#11030=DIRECTION('',(0.5,0.866025403784439,0.));
#11031=DIRECTION('',(0.5,0.866025403784439,0.));
#11032=DIRECTION('center_axis',(0.,0.,1.));
#11033=DIRECTION('ref_axis',(1.,0.,0.));
#11034=DIRECTION('center_axis',(0.,0.,1.));
#11035=DIRECTION('ref_axis',(1.,0.,0.));
#11036=DIRECTION('center_axis',(0.,0.,1.));
#11037=DIRECTION('ref_axis',(1.,0.,0.));
#11038=DIRECTION('center_axis',(0.,0.,1.));
#11039=DIRECTION('ref_axis',(1.,0.,0.));
#11040=DIRECTION('',(0.,0.,-1.));
#11041=DIRECTION('center_axis',(0.,0.,1.));
#11042=DIRECTION('ref_axis',(1.,0.,0.));
#11043=DIRECTION('center_axis',(0.,0.,1.));
#11044=DIRECTION('ref_axis',(1.,0.,0.));
#11045=DIRECTION('center_axis',(0.,0.,1.));
#11046=DIRECTION('ref_axis',(1.,0.,0.));
#11047=DIRECTION('axis',(0.,0.,1.));
#11048=DIRECTION('refdir',(1.,0.,0.));
#11049=DIRECTION('center_axis',(0.,0.,1.));
#11050=DIRECTION('ref_axis',(1.,0.,0.));
#11051=DIRECTION('',(0.,0.,-1.));
#11052=DIRECTION('center_axis',(0.,0.,-1.));
#11053=DIRECTION('ref_axis',(1.,0.,0.));
#11054=DIRECTION('center_axis',(0.,0.,1.));
#11055=DIRECTION('ref_axis',(1.,0.,0.));
#11056=DIRECTION('',(0.,0.,-1.));
#11057=DIRECTION('center_axis',(0.,0.,1.));
#11058=DIRECTION('ref_axis',(1.,0.,0.));
#11059=DIRECTION('',(0.,0.,-1.));
#11060=DIRECTION('center_axis',(0.,0.,1.));
#11061=DIRECTION('ref_axis',(1.,0.,0.));
#11062=DIRECTION('',(0.,0.,-1.));
#11063=DIRECTION('center_axis',(0.,0.,1.));
#11064=DIRECTION('ref_axis',(1.,0.,0.));
#11065=DIRECTION('',(0.,0.,-1.));
#11066=DIRECTION('center_axis',(0.,0.,1.));
#11067=DIRECTION('ref_axis',(1.,0.,0.));
#11068=DIRECTION('',(0.,0.,-1.));
#11069=DIRECTION('center_axis',(0.,0.,1.));
#11070=DIRECTION('ref_axis',(1.,0.,0.));
#11071=DIRECTION('',(0.,0.,-1.));
#11072=DIRECTION('center_axis',(0.,0.,1.));
#11073=DIRECTION('ref_axis',(1.,0.,0.));
#11074=DIRECTION('',(0.,0.,-1.));
#11075=DIRECTION('center_axis',(0.,0.,1.));
#11076=DIRECTION('ref_axis',(1.,0.,0.));
#11077=DIRECTION('',(0.,0.,-1.));
#11078=DIRECTION('center_axis',(0.,0.,1.));
#11079=DIRECTION('ref_axis',(1.,0.,0.));
#11080=DIRECTION('',(0.,0.,-1.));
#11081=DIRECTION('center_axis',(0.,0.,1.));
#11082=DIRECTION('ref_axis',(1.,0.,0.));
#11083=DIRECTION('',(0.,0.,-1.));
#11084=DIRECTION('center_axis',(0.,0.,1.));
#11085=DIRECTION('ref_axis',(0.997344302588954,-0.0728309144069492,0.));
#11086=DIRECTION('',(0.,0.,1.));
#11087=DIRECTION('center_axis',(0.,0.,-1.));
#11088=DIRECTION('ref_axis',(1.,7.52212518638754E-14,0.));
#11089=DIRECTION('center_axis',(0.,0.,1.));
#11090=DIRECTION('ref_axis',(1.,7.52212518638754E-14,0.));
#11091=DIRECTION('',(0.,0.,1.));
#11092=DIRECTION('center_axis',(0.,0.,1.));
#11093=DIRECTION('ref_axis',(1.,7.52212518638754E-14,0.));
#11094=DIRECTION('',(0.,0.,1.));
#11095=DIRECTION('center_axis',(0.,0.,1.));
#11096=DIRECTION('ref_axis',(1.,7.52212518638754E-14,0.));
#11097=DIRECTION('',(0.,0.,1.));
#11098=DIRECTION('center_axis',(0.,0.,1.));
#11099=DIRECTION('ref_axis',(1.,7.52212518638754E-14,0.));
#11100=DIRECTION('',(0.,0.,1.));
#11101=DIRECTION('center_axis',(0.,0.,1.));
#11102=DIRECTION('ref_axis',(1.,7.52212518638754E-14,0.));
#11103=DIRECTION('',(0.,0.,1.));
#11104=DIRECTION('center_axis',(0.,0.,1.));
#11105=DIRECTION('ref_axis',(1.,7.52212518638754E-14,0.));
#11106=DIRECTION('',(0.,0.,1.));
#11107=DIRECTION('center_axis',(0.,0.,1.));
#11108=DIRECTION('ref_axis',(1.,7.52212518638754E-14,0.));
#11109=DIRECTION('',(0.,0.,1.));
#11110=DIRECTION('center_axis',(0.,0.,1.));
#11111=DIRECTION('ref_axis',(1.,7.52212518638754E-14,0.));
#11112=DIRECTION('',(0.,0.,1.));
#11113=DIRECTION('center_axis',(0.,0.,1.));
#11114=DIRECTION('ref_axis',(1.,7.52212518638754E-14,0.));
#11115=DIRECTION('',(0.,0.,1.));
#11116=DIRECTION('center_axis',(0.,0.,1.));
#11117=DIRECTION('ref_axis',(1.,7.52212518638754E-14,0.));
#11118=DIRECTION('',(0.,0.,1.));
#11119=DIRECTION('center_axis',(0.,0.,-1.));
#11120=DIRECTION('ref_axis',(1.,0.,0.));
#11121=DIRECTION('center_axis',(0.,0.,-1.));
#11122=DIRECTION('ref_axis',(1.,0.,0.));
#11123=DIRECTION('',(0.707106781186548,8.65956056235494E-17,0.707106781186547));
#11124=DIRECTION('center_axis',(0.,0.,1.));
#11125=DIRECTION('ref_axis',(1.,0.,0.));
#11126=DIRECTION('center_axis',(0.,0.,1.));
#11127=DIRECTION('ref_axis',(1.,7.52212518638754E-14,0.));
#11128=DIRECTION('center_axis',(0.,0.,-1.));
#11129=DIRECTION('ref_axis',(1.,7.52212518638754E-14,0.));
#11130=DIRECTION('center_axis',(0.,0.,1.));
#11131=DIRECTION('ref_axis',(1.,0.,0.));
#11132=DIRECTION('center_axis',(-1.92296268638356E-16,-1.,0.));
#11133=DIRECTION('ref_axis',(1.,-1.92296268638356E-16,0.));
#11134=DIRECTION('',(1.,-1.92296268638356E-16,0.));
#11135=DIRECTION('',(0.,0.,1.));
#11136=DIRECTION('',(1.,-1.92296268638356E-16,0.));
#11137=DIRECTION('',(0.,0.,1.));
#11138=DIRECTION('center_axis',(-0.866025403784439,-0.5,0.));
#11139=DIRECTION('ref_axis',(0.5,-0.866025403784439,0.));
#11140=DIRECTION('',(0.5,-0.866025403784439,0.));
#11141=DIRECTION('',(0.,0.,1.));
#11142=DIRECTION('',(0.5,-0.866025403784439,0.));
#11143=DIRECTION('center_axis',(-0.866025403784439,0.5,0.));
#11144=DIRECTION('ref_axis',(-0.5,-0.866025403784438,0.));
#11145=DIRECTION('',(-0.5,-0.866025403784438,0.));
#11146=DIRECTION('',(0.,0.,1.));
#11147=DIRECTION('',(-0.5,-0.866025403784439,0.));
#11148=DIRECTION('center_axis',(1.92296268638356E-16,1.,0.));
#11149=DIRECTION('ref_axis',(-1.,1.92296268638356E-16,0.));
#11150=DIRECTION('',(-1.,1.92296268638356E-16,0.));
#11151=DIRECTION('',(0.,0.,1.));
#11152=DIRECTION('',(-1.,1.92296268638356E-16,0.));
#11153=DIRECTION('center_axis',(0.866025403784439,0.5,0.));
#11154=DIRECTION('ref_axis',(-0.5,0.866025403784439,0.));
#11155=DIRECTION('',(-0.5,0.866025403784439,0.));
#11156=DIRECTION('',(0.,0.,1.));
#11157=DIRECTION('',(-0.5,0.866025403784439,0.));
#11158=DIRECTION('center_axis',(0.866025403784439,-0.5,0.));
#11159=DIRECTION('ref_axis',(0.5,0.866025403784439,0.));
#11160=DIRECTION('',(0.5,0.866025403784439,0.));
#11161=DIRECTION('',(0.5,0.866025403784439,0.));
#11162=DIRECTION('center_axis',(0.,0.,1.));
#11163=DIRECTION('ref_axis',(1.,0.,0.));
#11164=DIRECTION('center_axis',(0.,0.,1.));
#11165=DIRECTION('ref_axis',(1.,0.,0.));
#11166=DIRECTION('center_axis',(0.,0.,1.));
#11167=DIRECTION('ref_axis',(1.,0.,0.));
#11168=DIRECTION('center_axis',(0.,0.,1.));
#11169=DIRECTION('ref_axis',(1.,0.,0.));
#11170=DIRECTION('',(0.,0.,-1.));
#11171=DIRECTION('center_axis',(0.,0.,1.));
#11172=DIRECTION('ref_axis',(1.,0.,0.));
#11173=DIRECTION('center_axis',(0.,0.,1.));
#11174=DIRECTION('ref_axis',(1.,0.,0.));
#11175=DIRECTION('center_axis',(0.,0.,1.));
#11176=DIRECTION('ref_axis',(1.,0.,0.));
#11177=DIRECTION('axis',(0.,0.,1.));
#11178=DIRECTION('refdir',(1.,0.,0.));
#11179=DIRECTION('center_axis',(0.,0.,1.));
#11180=DIRECTION('ref_axis',(1.,0.,0.));
#11181=DIRECTION('center_axis',(0.,0.,-1.));
#11182=DIRECTION('ref_axis',(1.,0.,0.));
#11183=DIRECTION('',(0.,0.,-1.));
#11184=DIRECTION('center_axis',(0.,0.,-1.));
#11185=DIRECTION('ref_axis',(1.,0.,0.));
#11186=DIRECTION('center_axis',(0.,0.,1.));
#11187=DIRECTION('ref_axis',(1.,0.,0.));
#11188=DIRECTION('center_axis',(0.,0.,1.));
#11189=DIRECTION('ref_axis',(1.,0.,0.));
#11190=DIRECTION('',(0.,0.,-1.));
#11191=DIRECTION('center_axis',(0.,0.,1.));
#11192=DIRECTION('ref_axis',(1.,0.,0.));
#11193=DIRECTION('center_axis',(0.,0.,1.));
#11194=DIRECTION('ref_axis',(1.,0.,0.));
#11195=DIRECTION('center_axis',(0.,0.,1.));
#11196=DIRECTION('ref_axis',(1.,0.,0.));
#11197=DIRECTION('axis',(0.,0.,1.));
#11198=DIRECTION('refdir',(1.,0.,0.));
#11199=DIRECTION('center_axis',(0.,0.,-1.));
#11200=DIRECTION('ref_axis',(-0.346824478021586,0.937930051467088,0.));
#11201=DIRECTION('',(0.,0.,-1.));
#11202=DIRECTION('center_axis',(0.,0.,-1.));
#11203=DIRECTION('ref_axis',(1.,0.,0.));
#11204=DIRECTION('center_axis',(0.,0.,-1.));
#11205=DIRECTION('ref_axis',(1.,0.,0.));
#11206=DIRECTION('',(0.,0.,-1.));
#11207=DIRECTION('center_axis',(0.,0.,-1.));
#11208=DIRECTION('ref_axis',(1.,0.,0.));
#11209=DIRECTION('',(0.,0.,-1.));
#11210=DIRECTION('center_axis',(0.,0.,-1.));
#11211=DIRECTION('ref_axis',(1.,0.,0.));
#11212=DIRECTION('',(0.,0.,-1.));
#11213=DIRECTION('center_axis',(0.,0.,-1.));
#11214=DIRECTION('ref_axis',(0.937996590358642,-0.346644481386278,0.));
#11215=DIRECTION('',(0.,0.,-1.));
#11216=DIRECTION('center_axis',(0.,0.,-1.));
#11217=DIRECTION('ref_axis',(1.,0.,0.));
#11218=DIRECTION('center_axis',(0.,0.,-1.));
#11219=DIRECTION('ref_axis',(0.7932173491397,0.608938615152452,0.));
#11220=DIRECTION('',(1.22464679914735E-16,-9.27389451825078E-31,-1.));
#11221=DIRECTION('center_axis',(0.,0.,1.));
#11222=DIRECTION('ref_axis',(1.,-7.45024487577726E-15,0.));
#11223=DIRECTION('center_axis',(0.,0.,-1.));
#11224=DIRECTION('ref_axis',(1.,-7.45024487577726E-15,0.));
#11225=DIRECTION('',(1.22464679914735E-16,-9.27389451825078E-31,-1.));
#11226=DIRECTION('center_axis',(0.,0.,-1.));
#11227=DIRECTION('ref_axis',(1.,-7.45024487577726E-15,0.));
#11228=DIRECTION('',(1.22464679914735E-16,-9.27389451825078E-31,-1.));
#11229=DIRECTION('center_axis',(0.,0.,-1.));
#11230=DIRECTION('ref_axis',(1.,-7.45024487577726E-15,0.));
#11231=DIRECTION('',(1.22464679914735E-16,-9.27389451825078E-31,-1.));
#11232=DIRECTION('center_axis',(0.,0.,-1.));
#11233=DIRECTION('ref_axis',(-0.609064819364946,-0.793120448489348,0.));
#11234=DIRECTION('',(1.22464679914735E-16,-9.27389451825078E-31,-1.));
#11235=DIRECTION('center_axis',(0.,0.,-1.));
#11236=DIRECTION('ref_axis',(1.,-7.45024487577726E-15,0.));
#11237=DIRECTION('center_axis',(0.,0.,-1.));
#11238=DIRECTION('ref_axis',(1.,-7.45024487577726E-15,0.));
#11239=DIRECTION('center_axis',(0.,0.,1.));
#11240=DIRECTION('ref_axis',(1.,0.,0.));
#11241=DIRECTION('',(0.5,0.866025403784439,0.));
#11242=DIRECTION('',(-0.5,0.866025403784439,0.));
#11243=DIRECTION('',(-1.,1.92296268638356E-16,0.));
#11244=DIRECTION('',(-0.5,-0.866025403784439,0.));
#11245=DIRECTION('',(0.5,-0.866025403784439,0.));
#11246=DIRECTION('',(1.,-1.92296268638356E-16,0.));
#11247=DIRECTION('center_axis',(0.,0.,-1.));
#11248=DIRECTION('ref_axis',(1.,0.,0.));
#11249=DIRECTION('center_axis',(-1.92296268638356E-16,-1.,0.));
#11250=DIRECTION('ref_axis',(1.,-1.92296268638356E-16,0.));
#11251=DIRECTION('',(1.,-1.92296268638356E-16,0.));
#11252=DIRECTION('',(0.,0.,1.));
#11253=DIRECTION('',(0.,0.,1.));
#11254=DIRECTION('center_axis',(-0.866025403784439,-0.5,0.));
#11255=DIRECTION('ref_axis',(0.5,-0.866025403784439,0.));
#11256=DIRECTION('',(0.5,-0.866025403784439,0.));
#11257=DIRECTION('',(0.,0.,1.));
#11258=DIRECTION('center_axis',(-0.866025403784439,0.5,0.));
#11259=DIRECTION('ref_axis',(-0.5,-0.866025403784438,0.));
#11260=DIRECTION('',(-0.5,-0.866025403784439,0.));
#11261=DIRECTION('',(0.,0.,1.));
#11262=DIRECTION('center_axis',(1.92296268638356E-16,1.,0.));
#11263=DIRECTION('ref_axis',(-1.,1.92296268638356E-16,0.));
#11264=DIRECTION('',(-1.,1.92296268638356E-16,0.));
#11265=DIRECTION('',(0.,0.,1.));
#11266=DIRECTION('center_axis',(0.866025403784439,0.5,0.));
#11267=DIRECTION('ref_axis',(-0.5,0.866025403784439,0.));
#11268=DIRECTION('',(-0.5,0.866025403784439,0.));
#11269=DIRECTION('',(0.,0.,1.));
#11270=DIRECTION('center_axis',(0.866025403784439,-0.5,0.));
#11271=DIRECTION('ref_axis',(0.5,0.866025403784439,0.));
#11272=DIRECTION('',(0.5,0.866025403784439,0.));
#11273=DIRECTION('center_axis',(0.,0.,1.));
#11274=DIRECTION('ref_axis',(1.,0.,0.));
#11275=DIRECTION('',(0.,0.,1.));
#11276=DIRECTION('',(1.,0.,0.));
#11277=DIRECTION('',(0.,0.,1.));
#11278=DIRECTION('',(1.,0.,0.));
#11279=DIRECTION('',(0.,0.,1.));
#11280=DIRECTION('',(1.,0.,0.));
#11281=DIRECTION('',(0.,0.,1.));
#11282=DIRECTION('',(1.,0.,0.));
#11283=DIRECTION('',(0.,0.,1.));
#11284=DIRECTION('',(1.,0.,0.));
#11285=DIRECTION('',(0.,1.,2.22044604925031E-16));
#11286=DIRECTION('',(1.,0.,0.));
#11287=DIRECTION('',(0.,1.,2.22044604925031E-16));
#11288=DIRECTION('',(1.,0.,0.));
#11289=DIRECTION('',(0.,0.,1.));
#11290=DIRECTION('',(1.,0.,0.));
#11291=DIRECTION('',(0.,0.,1.));
#11292=DIRECTION('',(-1.,1.22464679914735E-16,0.));
#11293=DIRECTION('',(0.,0.,1.));
#11294=DIRECTION('',(-1.,1.22464679914735E-16,0.));
#11295=DIRECTION('',(0.,0.,1.));
#11296=DIRECTION('',(1.,0.,0.));
#11297=DIRECTION('',(0.,0.,1.));
#11298=DIRECTION('',(1.,0.,0.));
#11299=DIRECTION('',(0.,0.,1.));
#11300=DIRECTION('',(1.,0.,0.));
#11301=DIRECTION('',(0.,0.,1.));
#11302=DIRECTION('',(1.,0.,0.));
#11303=DIRECTION('',(0.,0.,1.));
#11304=DIRECTION('',(1.,0.,0.));
#11305=DIRECTION('',(0.,0.,1.));
#11306=DIRECTION('',(1.,0.,0.));
#11307=DIRECTION('',(0.,0.,1.));
#11308=DIRECTION('',(1.,0.,0.));
#11309=DIRECTION('',(0.,-1.22464679914735E-16,-1.));
#11310=DIRECTION('',(-0.984807753012208,0.17364817766693,-2.12657684957577E-17));
#11311=DIRECTION('',(0.,0.,1.));
#11312=DIRECTION('',(1.,0.,0.));
#11313=DIRECTION('',(0.,1.,2.22044604925031E-16));
#11314=DIRECTION('',(1.,0.,0.));
#11315=DIRECTION('',(0.,1.,2.22044604925031E-16));
#11316=DIRECTION('',(1.,0.,0.));
#11317=DIRECTION('',(0.,0.,1.));
#11318=DIRECTION('',(1.,0.,0.));
#11319=DIRECTION('',(0.,0.,1.));
#11320=DIRECTION('',(1.,0.,0.));
#11321=DIRECTION('',(0.,0.,1.));
#11322=DIRECTION('',(-1.,1.22464679914735E-16,0.));
#11323=DIRECTION('',(0.,0.,1.));
#11324=DIRECTION('',(-1.,1.22464679914735E-16,0.));
#11325=DIRECTION('',(0.,0.,1.));
#11326=DIRECTION('',(1.,0.,0.));
#11327=DIRECTION('',(0.,0.,1.));
#11328=DIRECTION('',(1.,0.,0.));
#11329=DIRECTION('',(0.,0.,1.));
#11330=DIRECTION('',(1.,0.,0.));
#11331=DIRECTION('',(0.,0.,1.));
#11332=DIRECTION('',(-1.,1.22464679914735E-16,0.));
#11333=DIRECTION('',(0.,0.,1.));
#11334=DIRECTION('',(-1.,1.22464679914735E-16,0.));
#11335=DIRECTION('',(0.,0.,1.));
#11336=DIRECTION('',(1.,0.,0.));
#11337=DIRECTION('',(0.,0.,1.));
#11338=DIRECTION('',(1.,0.,0.));
#11339=DIRECTION('',(0.,0.,1.));
#11340=DIRECTION('',(1.,0.,0.));
#11341=DIRECTION('',(0.,0.,1.));
#11342=DIRECTION('',(-1.,1.22464679914735E-16,0.));
#11343=DIRECTION('',(0.,0.,1.));
#11344=DIRECTION('',(-1.,1.22464679914735E-16,0.));
#11345=DIRECTION('',(0.,0.,1.));
#11346=DIRECTION('',(1.,0.,0.));
#11347=DIRECTION('',(0.,0.,1.));
#11348=DIRECTION('',(1.,0.,0.));
#11349=CARTESIAN_POINT('',(0.,0.,0.));
#11350=CARTESIAN_POINT('',(0.,0.,0.));
#11351=CARTESIAN_POINT('Origin',(-205.,95.,9.));
#11352=CARTESIAN_POINT('',(-202.486487043593,95.0006372934558,16.612583302492));
#11353=CARTESIAN_POINT('',(-202.484597865978,94.9962675362615,16.887416697508));
#11354=CARTESIAN_POINT('',(-202.4825,95.,9.));
#11355=CARTESIAN_POINT('',(-203.086534003335,96.6359872033749,17.));
#11356=CARTESIAN_POINT('Ctrl Pts',(-202.484597865978,94.9962675362615,16.887416697508));
#11357=CARTESIAN_POINT('Ctrl Pts',(-202.48977981228,95.5889553626798,16.9249444650054));
#11358=CARTESIAN_POINT('Ctrl Pts',(-202.700778171916,96.1848035603043,16.9624722325027));
#11359=CARTESIAN_POINT('Ctrl Pts',(-203.086534003335,96.6359872033749,17.));
#11360=CARTESIAN_POINT('',(-202.4825,95.,17.));
#11361=CARTESIAN_POINT('Origin',(-205.,95.,17.));
#11362=CARTESIAN_POINT('',(-202.4825,95.,18.));
#11363=CARTESIAN_POINT('',(-202.4825,95.,9.));
#11364=CARTESIAN_POINT('Origin',(-205.,95.,18.));
#11365=CARTESIAN_POINT('',(-206.917150800208,96.6387883530143,17.));
#11366=CARTESIAN_POINT('Origin',(-205.,95.,17.));
#11367=CARTESIAN_POINT('Ctrl Pts',(-206.917153830491,96.638790656604,17.));
#11368=CARTESIAN_POINT('Ctrl Pts',(-206.385184906259,97.2593583513323,16.9480939310855));
#11369=CARTESIAN_POINT('Ctrl Pts',(-205.522590916198,97.5988876213873,16.896187862171));
#11370=CARTESIAN_POINT('Ctrl Pts',(-204.710520946275,97.5049655781755,16.8442817932565));
#11371=CARTESIAN_POINT('Ctrl Pts',(-203.881814551752,97.4091194064428,16.7913123536551));
#11372=CARTESIAN_POINT('Ctrl Pts',(-203.105723496861,96.8618802537328,16.7383429140536));
#11373=CARTESIAN_POINT('Ctrl Pts',(-202.737493201107,96.1136066926246,16.6853734744522));
#11374=CARTESIAN_POINT('Ctrl Pts',(-202.568820177878,95.7708495506689,16.6611100837988));
#11375=CARTESIAN_POINT('Ctrl Pts',(-202.485725551784,95.3859108502911,16.6368466931454));
#11376=CARTESIAN_POINT('Ctrl Pts',(-202.486487043593,95.0006372934558,16.612583302492));
#11377=CARTESIAN_POINT('Origin',(-205.,95.,9.));
#11378=CARTESIAN_POINT('',(-202.482805429294,94.9976897526833,15.612583302492));
#11379=CARTESIAN_POINT('',(-202.478254054321,95.0000324001602,15.887416697508));
#11380=CARTESIAN_POINT('',(-202.4825,95.,9.));
#11381=CARTESIAN_POINT('Ctrl Pts',(-202.478254054321,95.0000324001602,15.887416697508));
#11382=CARTESIAN_POINT('Ctrl Pts',(-202.4781431837,95.835267846479,15.9404611607301));
#11383=CARTESIAN_POINT('Ctrl Pts',(-202.934422716347,96.6703686768054,15.9935056239521));
#11384=CARTESIAN_POINT('Ctrl Pts',(-203.637201874695,97.1217724188669,16.0465500871742));
#11385=CARTESIAN_POINT('Ctrl Pts',(-204.338987054902,97.5725377164795,16.0995195267756));
#11386=CARTESIAN_POINT('Ctrl Pts',(-205.286574244665,97.6406905263686,16.152488966377));
#11387=CARTESIAN_POINT('Ctrl Pts',(-206.045561328886,97.294827824976,16.2054584059785));
#11388=CARTESIAN_POINT('Ctrl Pts',(-206.804548413106,96.9489651235833,16.2584278455799));
#11389=CARTESIAN_POINT('Ctrl Pts',(-207.374935391785,96.189086910909,16.3113972851814));
#11390=CARTESIAN_POINT('Ctrl Pts',(-207.495329285435,95.3638523036021,16.3643667247828));
#11391=CARTESIAN_POINT('Ctrl Pts',(-207.615723179085,94.5386176962952,16.4173361643842));
#11392=CARTESIAN_POINT('Ctrl Pts',(-207.286123987708,93.6480266943556,16.4703056039857));
#11393=CARTESIAN_POINT('Ctrl Pts',(-206.657476699318,93.0996259784246,16.5232750435871));
#11394=CARTESIAN_POINT('Ctrl Pts',(-206.028829410928,92.5512252624936,16.5762444831885));
#11395=CARTESIAN_POINT('Ctrl Pts',(-205.101134025526,92.3450148325712,16.62921392279));
#11396=CARTESIAN_POINT('Ctrl Pts',(-204.299947458499,92.576953621889,16.6821833623914));
#11397=CARTESIAN_POINT('Ctrl Pts',(-203.498760891472,92.8088924112068,16.7351528019928));
#11398=CARTESIAN_POINT('Ctrl Pts',(-202.824083142821,93.4789804197649,16.7881222415943));
#11399=CARTESIAN_POINT('Ctrl Pts',(-202.584905412425,94.2765457081108,16.8410916811957));
#11400=CARTESIAN_POINT('Ctrl Pts',(-202.515180225313,94.5090522582447,16.8565333532998));
#11401=CARTESIAN_POINT('Ctrl Pts',(-202.482465633741,94.7523923556688,16.8719750254039));
#11402=CARTESIAN_POINT('Ctrl Pts',(-202.484597865978,94.9962675362615,16.887416697508));
#11403=CARTESIAN_POINT('Ctrl Pts',(-202.486487043593,95.0006372934558,16.612583302492));
#11404=CARTESIAN_POINT('Ctrl Pts',(-202.48738796554,94.5448196487217,16.583877253544));
#11405=CARTESIAN_POINT('Ctrl Pts',(-202.605664700594,94.0885332958007,16.5551712045959));
#11406=CARTESIAN_POINT('Ctrl Pts',(-202.838465118499,93.7010772441806,16.5264651556479));
#11407=CARTESIAN_POINT('Ctrl Pts',(-203.268036868263,92.9861293263514,16.4734957160465));
#11408=CARTESIAN_POINT('Ctrl Pts',(-204.087549904409,92.5055414601994,16.420526276445));
#11409=CARTESIAN_POINT('Ctrl Pts',(-204.921224621725,92.4794977627324,16.3675568368436));
#11410=CARTESIAN_POINT('Ctrl Pts',(-205.754899339041,92.4534540652654,16.3145873972421));
#11411=CARTESIAN_POINT('Ctrl Pts',(-206.602735737526,92.8819545364836,16.2616179576407));
#11412=CARTESIAN_POINT('Ctrl Pts',(-207.076148107766,93.5686324160268,16.2086485180393));
#11413=CARTESIAN_POINT('Ctrl Pts',(-207.549560478006,94.2553102955701,16.1556790784378));
#11414=CARTESIAN_POINT('Ctrl Pts',(-207.64854882,95.2001655834383,16.1027096388364));
#11415=CARTESIAN_POINT('Ctrl Pts',(-207.327709494231,95.970055069638,16.049740199235));
#11416=CARTESIAN_POINT('Ctrl Pts',(-207.006870168461,96.7399445558378,15.9967707596335));
#11417=CARTESIAN_POINT('Ctrl Pts',(-206.266203174927,97.3348682403689,15.9438013200321));
#11418=CARTESIAN_POINT('Ctrl Pts',(-205.445239637068,97.4821294064964,15.8908318804307));
#11419=CARTESIAN_POINT('Ctrl Pts',(-204.624276099208,97.6293905726238,15.8378624408292));
#11420=CARTESIAN_POINT('Ctrl Pts',(-203.723016017023,97.3289892203476,15.7848930012278));
#11421=CARTESIAN_POINT('Ctrl Pts',(-203.154585439598,96.7186213746173,15.7319235616264));
#11422=CARTESIAN_POINT('Ctrl Pts',(-202.727693676347,96.260234693386,15.6921434752482));
#11423=CARTESIAN_POINT('Ctrl Pts',(-202.488518438045,95.6270262725852,15.6523633888701));
#11424=CARTESIAN_POINT('Ctrl Pts',(-202.482805429294,94.9976897526833,15.612583302492));
#11425=CARTESIAN_POINT('Origin',(-205.,95.,9.));
#11426=CARTESIAN_POINT('',(-202.47847166618,95.0006753796333,14.612583302492));
#11427=CARTESIAN_POINT('',(-202.483904416421,95.0021895168216,14.887416697508));
#11428=CARTESIAN_POINT('',(-202.4825,95.,9.));
#11429=CARTESIAN_POINT('Ctrl Pts',(-202.483904416421,95.0021895168216,14.887416697508));
#11430=CARTESIAN_POINT('Ctrl Pts',(-202.481855095851,95.2491301525216,14.9030084168534));
#11431=CARTESIAN_POINT('Ctrl Pts',(-202.515258340335,95.4955283668393,14.9186001361987));
#11432=CARTESIAN_POINT('Ctrl Pts',(-202.586378614567,95.7305110407181,14.934191855544));
#11433=CARTESIAN_POINT('Ctrl Pts',(-202.82799411488,96.5288130288264,14.9871612951455));
#11434=CARTESIAN_POINT('Ctrl Pts',(-203.504921198234,97.1953624104036,15.0401307347469));
#11435=CARTESIAN_POINT('Ctrl Pts',(-204.306860479768,97.4246176783161,15.0931001743483));
#11436=CARTESIAN_POINT('Ctrl Pts',(-205.108799761302,97.6538729462285,15.1460696139498));
#11437=CARTESIAN_POINT('Ctrl Pts',(-206.035751241016,97.4458341004763,15.1990390535512));
#11438=CARTESIAN_POINT('Ctrl Pts',(-206.662805112391,96.8958629087621,15.2520084931526));
#11439=CARTESIAN_POINT('Ctrl Pts',(-207.289858983766,96.3458917170479,15.3049779327541));
#11440=CARTESIAN_POINT('Ctrl Pts',(-207.617015246803,95.4539881793718,15.3579473723555));
#11441=CARTESIAN_POINT('Ctrl Pts',(-207.494308184462,94.6290001862474,15.4109168119569));
#11442=CARTESIAN_POINT('Ctrl Pts',(-207.37160112212,93.8040121931229,15.4638862515584));
#11443=CARTESIAN_POINT('Ctrl Pts',(-206.799030734401,93.0459397445501,15.5168556911598));
#11444=CARTESIAN_POINT('Ctrl Pts',(-206.039058256267,92.7022701388405,15.5698251307613));
#11445=CARTESIAN_POINT('Ctrl Pts',(-205.279085778134,92.3586005331309,15.6227945703627));
#11446=CARTESIAN_POINT('Ctrl Pts',(-204.331711209586,92.4293337702846,15.6757640099641));
#11447=CARTESIAN_POINT('Ctrl Pts',(-203.631209544004,92.8820644793853,15.7287334495656));
#11448=CARTESIAN_POINT('Ctrl Pts',(-202.931700038648,93.3341539603135,15.7816278655464));
#11449=CARTESIAN_POINT('Ctrl Pts',(-202.478364611322,94.1671595901444,15.8345222815272));
#11450=CARTESIAN_POINT('Ctrl Pts',(-202.478254054321,95.0000324001602,15.887416697508));
#11451=CARTESIAN_POINT('Ctrl Pts',(-202.482805429294,94.9976897526833,15.612583302492));
#11452=CARTESIAN_POINT('Ctrl Pts',(-202.480911243101,94.7890290278569,15.5993939492687));
#11453=CARTESIAN_POINT('Ctrl Pts',(-202.504681520023,94.5807939404367,15.5862045960454));
#11454=CARTESIAN_POINT('Ctrl Pts',(-202.55578359808,94.3794975106792,15.5730152428221));
#11455=CARTESIAN_POINT('Ctrl Pts',(-202.761013406651,93.5710758316558,15.5200458032206));
#11456=CARTESIAN_POINT('Ctrl Pts',(-203.407074096456,92.8745668127933,15.4670763636192));
#11457=CARTESIAN_POINT('Ctrl Pts',(-204.197813528595,92.6092448276169,15.4141069240178));
#11458=CARTESIAN_POINT('Ctrl Pts',(-204.988552960733,92.3439228424405,15.3611374844163));
#11459=CARTESIAN_POINT('Ctrl Pts',(-205.923971135204,92.5097878909503,15.3081680448149));
#11460=CARTESIAN_POINT('Ctrl Pts',(-206.575278327948,93.0308090720576,15.2551986052134));
#11461=CARTESIAN_POINT('Ctrl Pts',(-207.226585520692,93.551830253165,15.202229165612));
#11462=CARTESIAN_POINT('Ctrl Pts',(-207.593781731709,94.4280075668699,15.1492597260106));
#11463=CARTESIAN_POINT('Ctrl Pts',(-207.508545912156,95.2577058854654,15.0962902864091));
#11464=CARTESIAN_POINT('Ctrl Pts',(-207.423310092601,96.0874042040608,15.0433208468077));
#11465=CARTESIAN_POINT('Ctrl Pts',(-206.885642242476,96.8706235275468,14.9903514072063));
#11466=CARTESIAN_POINT('Ctrl Pts',(-206.142006472617,97.2483406611404,14.9373819676048));
#11467=CARTESIAN_POINT('Ctrl Pts',(-205.398370702758,97.626057794734,14.8844125280034));
#11468=CARTESIAN_POINT('Ctrl Pts',(-204.448767013166,97.5982727384352,14.831443088402));
#11469=CARTESIAN_POINT('Ctrl Pts',(-203.728488344688,97.177721926406,14.7784736488005));
#11470=CARTESIAN_POINT('Ctrl Pts',(-203.008209676211,96.7571711143768,14.7255042091991));
#11471=CARTESIAN_POINT('Ctrl Pts',(-202.517256028848,95.9438545466172,14.6725347695977));
#11472=CARTESIAN_POINT('Ctrl Pts',(-202.480677851392,95.1105920315276,14.6195653299962));
#11473=CARTESIAN_POINT('Ctrl Pts',(-202.479070699274,95.0739805951826,14.6172379874948));
#11474=CARTESIAN_POINT('Ctrl Pts',(-202.47834071908,95.0373306531828,14.6149106449934));
#11475=CARTESIAN_POINT('Ctrl Pts',(-202.47847166618,95.0006753796333,14.612583302492));
#11476=CARTESIAN_POINT('Origin',(-205.,95.,9.));
#11477=CARTESIAN_POINT('',(-202.484820331358,95.0019240783679,13.612583302492));
#11478=CARTESIAN_POINT('',(-202.48602791266,94.998843140303,13.887416697508));
#11479=CARTESIAN_POINT('',(-202.4825,95.,9.));
#11480=CARTESIAN_POINT('Ctrl Pts',(-202.48602791266,94.998843140303,13.887416697508));
#11481=CARTESIAN_POINT('Ctrl Pts',(-202.488072688334,95.4925836353709,13.9185251125781));
#11482=CARTESIAN_POINT('Ctrl Pts',(-202.628459938899,95.9873972957536,13.9496335276481));
#11483=CARTESIAN_POINT('Ctrl Pts',(-202.899511357491,96.3954074594928,13.9807419427182));
#11484=CARTESIAN_POINT('Ctrl Pts',(-203.361040551879,97.0901413337929,14.0337113823196));
#11485=CARTESIAN_POINT('Ctrl Pts',(-204.201405965845,97.5332047692011,14.0866808219211));
#11486=CARTESIAN_POINT('Ctrl Pts',(-205.035388792576,97.521499975804,14.1396502615225));
#11487=CARTESIAN_POINT('Ctrl Pts',(-205.869371619307,97.509795182407,14.1926197011239));
#11488=CARTESIAN_POINT('Ctrl Pts',(-206.696971858804,97.0433221602047,14.2455891407254));
#11489=CARTESIAN_POINT('Ctrl Pts',(-207.138822180752,96.335909509144,14.2985585803268));
#11490=CARTESIAN_POINT('Ctrl Pts',(-207.580672502701,95.6284968580833,14.3515280199282));
#11491=CARTESIAN_POINT('Ctrl Pts',(-207.636772907101,94.6801445781641,14.4044974595297));
#11492=CARTESIAN_POINT('Ctrl Pts',(-207.281407293431,93.9255721097145,14.4574668991311));
#11493=CARTESIAN_POINT('Ctrl Pts',(-206.92604167976,93.1709996412648,14.5104363387325));
#11494=CARTESIAN_POINT('Ctrl Pts',(-206.159210048017,92.6102069842847,14.563405778334));
#11495=CARTESIAN_POINT('Ctrl Pts',(-205.332423709386,92.5002582451323,14.6163752179354));
#11496=CARTESIAN_POINT('Ctrl Pts',(-204.505637370754,92.3903095059799,14.6693446575369));
#11497=CARTESIAN_POINT('Ctrl Pts',(-203.618896325232,92.7312046846553,14.7223140971383));
#11498=CARTESIAN_POINT('Ctrl Pts',(-203.078677761108,93.3666795713128,14.7752835367397));
#11499=CARTESIAN_POINT('Ctrl Pts',(-202.697474212062,93.8151004479916,14.8126612569958));
#11500=CARTESIAN_POINT('Ctrl Pts',(-202.488817212071,94.410203617343,14.8500389772519));
#11501=CARTESIAN_POINT('Ctrl Pts',(-202.483904416421,95.0021895168216,14.887416697508));
#11502=CARTESIAN_POINT('Ctrl Pts',(-202.47847166618,95.0006753796333,14.612583302492));
#11503=CARTESIAN_POINT('Ctrl Pts',(-202.481321025821,94.2030704198136,14.561941205392));
#11504=CARTESIAN_POINT('Ctrl Pts',(-202.891803295554,93.402941071284,14.5112991082919));
#11505=CARTESIAN_POINT('Ctrl Pts',(-203.542553765119,92.9420726165712,14.4606570111919));
#11506=CARTESIAN_POINT('Ctrl Pts',(-204.223210563852,92.4600241791239,14.4076875715905));
#11507=CARTESIAN_POINT('Ctrl Pts',(-205.166726868867,92.3491357666491,14.354718131989));
#11508=CARTESIAN_POINT('Ctrl Pts',(-205.940600088161,92.6602380168317,14.3017486923876));
#11509=CARTESIAN_POINT('Ctrl Pts',(-206.714473307454,92.9713402670144,14.2487792527862));
#11510=CARTESIAN_POINT('Ctrl Pts',(-207.318703441026,93.7044331798545,14.1958098131847));
#11511=CARTESIAN_POINT('Ctrl Pts',(-207.476314767743,94.523471056521,14.1428403735833));
#11512=CARTESIAN_POINT('Ctrl Pts',(-207.63392609446,95.3425089331874,14.0898709339819));
#11513=CARTESIAN_POINT('Ctrl Pts',(-207.344918614323,96.2474917736803,14.0369014943804));
#11514=CARTESIAN_POINT('Ctrl Pts',(-206.741771743353,96.8235805034484,13.983932054779));
#11515=CARTESIAN_POINT('Ctrl Pts',(-206.138624872383,97.3996692332166,13.9309626151776));
#11516=CARTESIAN_POINT('Ctrl Pts',(-205.221338610581,97.64686385226,13.8779931755761));
#11517=CARTESIAN_POINT('Ctrl Pts',(-204.410391853126,97.4518517276016,13.8250237359747));
#11518=CARTESIAN_POINT('Ctrl Pts',(-203.599445095671,97.2568396029432,13.7720542963732));
#11519=CARTESIAN_POINT('Ctrl Pts',(-202.894837842562,96.619620734583,13.7190848567718));
#11520=CARTESIAN_POINT('Ctrl Pts',(-202.619558121519,95.8322926912433,13.6661154171704));
#11521=CARTESIAN_POINT('Ctrl Pts',(-202.526823482411,95.5670621770531,13.6482713789442));
#11522=CARTESIAN_POINT('Ctrl Pts',(-202.482810749722,95.2847966380167,13.6304273407181));
#11523=CARTESIAN_POINT('Ctrl Pts',(-202.484820331358,95.0019240783679,13.612583302492));
#11524=CARTESIAN_POINT('Origin',(-205.,95.,9.));
#11525=CARTESIAN_POINT('',(-202.485427355471,94.9983727942933,12.612583302492));
#11526=CARTESIAN_POINT('',(-202.479664315357,94.9983441169425,12.887416697508));
#11527=CARTESIAN_POINT('',(-202.4825,95.,9.));
#11528=CARTESIAN_POINT('Ctrl Pts',(-202.479664315357,94.9983441169425,12.887416697508));
#11529=CARTESIAN_POINT('Ctrl Pts',(-202.485253167408,95.7336004827625,12.9340418083028));
#11530=CARTESIAN_POINT('Ctrl Pts',(-202.825737604096,96.473362659355,12.9806669190976));
#11531=CARTESIAN_POINT('Ctrl Pts',(-203.391055625289,96.9417807577727,13.0272920298924));
#11532=CARTESIAN_POINT('Ctrl Pts',(-204.033297075631,97.4739370089732,13.0802614694938));
#11533=CARTESIAN_POINT('Ctrl Pts',(-204.965721673696,97.6558809958686,13.1332309090952));
#11534=CARTESIAN_POINT('Ctrl Pts',(-205.760911194526,97.4042106118059,13.1862003486967));
#11535=CARTESIAN_POINT('Ctrl Pts',(-206.556100715355,97.1525402277431,13.2391697882981));
#11536=CARTESIAN_POINT('Ctrl Pts',(-207.214055158948,96.4672554727222,13.2921392278995));
#11537=CARTESIAN_POINT('Ctrl Pts',(-207.433171885202,95.6624870484612,13.345108667501));
#11538=CARTESIAN_POINT('Ctrl Pts',(-207.652288611455,94.8577186242001,13.3980781071024));
#11539=CARTESIAN_POINT('Ctrl Pts',(-207.432567620369,93.9334665306991,13.4510475467038));
#11540=CARTESIAN_POINT('Ctrl Pts',(-206.874727786515,93.3134027632356,13.5040169863053));
#11541=CARTESIAN_POINT('Ctrl Pts',(-206.316887952661,92.6933389957721,13.5569864259067));
#11542=CARTESIAN_POINT('Ctrl Pts',(-205.420929276038,92.3774635543461,13.6099558655081));
#11543=CARTESIAN_POINT('Ctrl Pts',(-204.597554206738,92.5105719746145,13.6629253051096));
#11544=CARTESIAN_POINT('Ctrl Pts',(-203.774179137438,92.6436803948829,13.715894744711));
#11545=CARTESIAN_POINT('Ctrl Pts',(-203.023387675461,93.2257726768456,13.7688641843124));
#11546=CARTESIAN_POINT('Ctrl Pts',(-202.689338431877,93.990020974423,13.8218336239139));
#11547=CARTESIAN_POINT('Ctrl Pts',(-202.551472923697,94.3054339919501,13.8436946484453));
#11548=CARTESIAN_POINT('Ctrl Pts',(-202.484590973778,94.6518735807638,13.8655556729767));
#11549=CARTESIAN_POINT('Ctrl Pts',(-202.48602791266,94.998843140303,13.887416697508));
#11550=CARTESIAN_POINT('Ctrl Pts',(-202.484820331358,95.0019240783679,13.612583302492));
#11551=CARTESIAN_POINT('Ctrl Pts',(-202.488776126603,94.4450987639516,13.5774579011167));
#11552=CARTESIAN_POINT('Ctrl Pts',(-202.671062063926,93.8859213280996,13.5423324997414));
#11553=CARTESIAN_POINT('Ctrl Pts',(-203.011086898641,93.4496970181517,13.5072070983661));
#11554=CARTESIAN_POINT('Ctrl Pts',(-203.523847585785,92.7918666067188,13.4542376587646));
#11555=CARTESIAN_POINT('Ctrl Pts',(-204.395321149052,92.4136430021722,13.4012682191632));
#11556=CARTESIAN_POINT('Ctrl Pts',(-205.2260289773,92.4884017912889,13.3482987795618));
#11557=CARTESIAN_POINT('Ctrl Pts',(-206.056736805549,92.5631605804057,13.2953293399603));
#11558=CARTESIAN_POINT('Ctrl Pts',(-206.84667889878,93.0909017631857,13.2423599003589));
#11559=CARTESIAN_POINT('Ctrl Pts',(-207.233750215907,93.8297117306135,13.1893904607575));
#11560=CARTESIAN_POINT('Ctrl Pts',(-207.620821533034,94.5685216980413,13.136421021156));
#11561=CARTESIAN_POINT('Ctrl Pts',(-207.605022074058,95.5184004501168,13.0834515815546));
#11562=CARTESIAN_POINT('Ctrl Pts',(-207.193594222707,96.2439288752151,13.0304821419532));
#11563=CARTESIAN_POINT('Ctrl Pts',(-206.782166371356,96.9694573003133,12.9775127023517));
#11564=CARTESIAN_POINT('Ctrl Pts',(-205.975110127631,97.4706353984343,12.9245432627503));
#11565=CARTESIAN_POINT('Ctrl Pts',(-205.142375563491,97.5177259301682,12.8715738231488));
#11566=CARTESIAN_POINT('Ctrl Pts',(-204.309640999352,97.564816461902,12.8186043835474));
#11567=CARTESIAN_POINT('Ctrl Pts',(-203.451228114797,97.1578194272488,12.765634943946));
#11568=CARTESIAN_POINT('Ctrl Pts',(-202.960628578963,96.483299992439,12.7126655043445));
#11569=CARTESIAN_POINT('Ctrl Pts',(-202.65164361113,96.058480255272,12.6793047703937));
#11570=CARTESIAN_POINT('Ctrl Pts',(-202.488556167955,95.5275445869965,12.6459440364428));
#11571=CARTESIAN_POINT('Ctrl Pts',(-202.485427355471,94.9983727942933,12.612583302492));
#11572=CARTESIAN_POINT('Origin',(-205.,95.,9.));
#11573=CARTESIAN_POINT('',(-202.478890863588,94.9988537196689,11.612583302492));
#11574=CARTESIAN_POINT('',(-202.480886672631,95.0021035940924,11.887416697508));
#11575=CARTESIAN_POINT('',(-202.4825,95.,9.));
#11576=CARTESIAN_POINT('Ctrl Pts',(-202.480886672631,95.0021035940924,11.887416697508));
#11577=CARTESIAN_POINT('Ctrl Pts',(-202.479589474908,95.146930289923,11.8965890644261));
#11578=CARTESIAN_POINT('Ctrl Pts',(-202.491001904373,95.2915526532226,11.9057614313441));
#11579=CARTESIAN_POINT('Ctrl Pts',(-202.515848826212,95.4338288347626,11.9149337982622));
#11580=CARTESIAN_POINT('Ctrl Pts',(-202.659337146883,96.2554585920688,11.9679032378636));
#11581=CARTESIAN_POINT('Ctrl Pts',(-203.250857617326,96.998844614645,12.0208726774651));
#11582=CARTESIAN_POINT('Ctrl Pts',(-204.019260559541,97.3232229040773,12.0738421170665));
#11583=CARTESIAN_POINT('Ctrl Pts',(-204.787663501755,97.6476011935096,12.1268115566679));
#11584=CARTESIAN_POINT('Ctrl Pts',(-205.732948915742,97.552971749798,12.1797809962694));
#11585=CARTESIAN_POINT('Ctrl Pts',(-206.42180325036,97.0827121811151,12.2327504358708));
#11586=CARTESIAN_POINT('Ctrl Pts',(-207.110657584977,96.6124526124322,12.2857198754723));
#11587=CARTESIAN_POINT('Ctrl Pts',(-207.543080840225,95.766562918778,12.3386893150737));
#11588=CARTESIAN_POINT('Ctrl Pts',(-207.52085261245,94.932794208552,12.3916587546751));
#11589=CARTESIAN_POINT('Ctrl Pts',(-207.498624384675,94.0990254983261,12.4446281942766));
#11590=CARTESIAN_POINT('Ctrl Pts',(-207.021744673877,93.2773777715286,12.497597633878));
#11591=CARTESIAN_POINT('Ctrl Pts',(-206.308812474494,92.844489754439,12.5505670734794));
#11592=CARTESIAN_POINT('Ctrl Pts',(-205.595880275112,92.4116017373494,12.6035365130809));
#11593=CARTESIAN_POINT('Ctrl Pts',(-204.646895587144,92.3674734299677,12.6565059526823));
#11594=CARTESIAN_POINT('Ctrl Pts',(-203.89686768825,92.7323330017727,12.7094753922837));
#11595=CARTESIAN_POINT('Ctrl Pts',(-203.146839789356,93.0971925735776,12.7624448318852));
#11596=CARTESIAN_POINT('Ctrl Pts',(-202.595768679535,93.8710400245692,12.8154142714866));
#11597=CARTESIAN_POINT('Ctrl Pts',(-202.496262275933,94.6991480078178,12.868383711088));
#11598=CARTESIAN_POINT('Ctrl Pts',(-202.484344057662,94.7983332998029,12.8747280398947));
#11599=CARTESIAN_POINT('Ctrl Pts',(-202.478903834267,94.8982969950711,12.8810723687014));
#11600=CARTESIAN_POINT('Ctrl Pts',(-202.479664315357,94.9983441169425,12.887416697508));
#11601=CARTESIAN_POINT('Ctrl Pts',(-202.485427355471,94.9983727942933,12.612583302492));
#11602=CARTESIAN_POINT('Ctrl Pts',(-202.483588308311,94.6873372536185,12.5929745968414));
#11603=CARTESIAN_POINT('Ctrl Pts',(-202.537012246085,94.3769111019385,12.5733658911908));
#11604=CARTESIAN_POINT('Ctrl Pts',(-202.648554519612,94.0890012001821,12.5537571855402));
#11605=CARTESIAN_POINT('Ctrl Pts',(-202.949866183209,93.3112636777014,12.5007877459388));
#11606=CARTESIAN_POINT('Ctrl Pts',(-203.675275697519,92.6978304677061,12.4478183063374));
#11607=CARTESIAN_POINT('Ctrl Pts',(-204.492259395059,92.5298959255516,12.3948488667359));
#11608=CARTESIAN_POINT('Ctrl Pts',(-205.309243092599,92.3619613833971,12.3418794271345));
#11609=CARTESIAN_POINT('Ctrl Pts',(-206.217800973369,92.6395255090834,12.2889099875331));
#11610=CARTESIAN_POINT('Ctrl Pts',(-206.801455182205,93.2353544585335,12.2359405479316));
#11611=CARTESIAN_POINT('Ctrl Pts',(-207.385109391041,93.8311834079836,12.1829711083302));
#11612=CARTESIAN_POINT('Ctrl Pts',(-207.643859927944,94.7452771811977,12.1300016687287));
#11613=CARTESIAN_POINT('Ctrl Pts',(-207.459096992797,95.5586203008532,12.0770322291273));
#11614=CARTESIAN_POINT('Ctrl Pts',(-207.274334057651,96.3719634205086,12.0240627895259));
#11615=CARTESIAN_POINT('Ctrl Pts',(-206.646057650456,97.0845558866056,11.9710933499244));
#11616=CARTESIAN_POINT('Ctrl Pts',(-205.862266165212,97.3697492949344,11.918123910323));
#11617=CARTESIAN_POINT('Ctrl Pts',(-205.078474679968,97.6549427032632,11.8651544707216));
#11618=CARTESIAN_POINT('Ctrl Pts',(-204.139168116676,97.5127370538238,11.8121850311201));
#11619=CARTESIAN_POINT('Ctrl Pts',(-203.474919354731,97.0083186216177,11.7592155915187));
#11620=CARTESIAN_POINT('Ctrl Pts',(-202.86198532346,96.5428676628624,11.7103381618431));
#11621=CARTESIAN_POINT('Ctrl Pts',(-202.483252930993,95.7690057922765,11.6614607321676));
#11622=CARTESIAN_POINT('Ctrl Pts',(-202.478890863588,94.9988537196689,11.612583302492));
#11623=CARTESIAN_POINT('Origin',(-205.,95.,9.));
#11624=CARTESIAN_POINT('',(-202.481958520358,95.002283592634,10.612583302492));
#11625=CARTESIAN_POINT('',(-202.486464188569,95.0004666863557,10.887416697508));
#11626=CARTESIAN_POINT('',(-202.4825,95.,9.));
#11627=CARTESIAN_POINT('Ctrl Pts',(-202.486464188569,95.0004666863557,10.887416697508));
#11628=CARTESIAN_POINT('Ctrl Pts',(-202.485815967357,95.3924916278335,10.9121057601508));
#11629=CARTESIAN_POINT('Ctrl Pts',(-202.571975294708,95.7842468732566,10.9367948227936));
#11630=CARTESIAN_POINT('Ctrl Pts',(-202.746434438658,96.1316610680036,10.9614838854364));
#11631=CARTESIAN_POINT('Ctrl Pts',(-203.12072985935,96.8770249350567,11.0144533250378));
#11632=CARTESIAN_POINT('Ctrl Pts',(-203.901469877197,97.4182866740021,11.0674227646392));
#11633=CARTESIAN_POINT('Ctrl Pts',(-204.730767631102,97.5073349284926,11.1203922042407));
#11634=CARTESIAN_POINT('Ctrl Pts',(-205.560065385007,97.5963831829831,11.1733616438421));
#11635=CARTESIAN_POINT('Ctrl Pts',(-206.437920874971,97.2332179530186,11.2263310834435));
#11636=CARTESIAN_POINT('Ctrl Pts',(-206.961930050197,96.5843121505036,11.279300523045));
#11637=CARTESIAN_POINT('Ctrl Pts',(-207.485939225424,95.9354063479886,11.3322699626464));
#11638=CARTESIAN_POINT('Ctrl Pts',(-207.656102085915,95.000759972923,11.3852394022478));
#11639=CARTESIAN_POINT('Ctrl Pts',(-207.394416927358,94.2088097004623,11.4382088418493));
#11640=CARTESIAN_POINT('Ctrl Pts',(-207.132731768801,93.4168594280015,11.4911782814507));
#11641=CARTESIAN_POINT('Ctrl Pts',(-206.439198591197,92.7676052581456,11.5441477210522));
#11642=CARTESIAN_POINT('Ctrl Pts',(-205.63172912742,92.5586616740667,11.5971171606536));
#11643=CARTESIAN_POINT('Ctrl Pts',(-204.824259663643,92.3497180899878,11.650086600255));
#11644=CARTESIAN_POINT('Ctrl Pts',(-203.902853913694,92.581085091686,11.7030560398565));
#11645=CARTESIAN_POINT('Ctrl Pts',(-203.289879124169,93.1467053385531,11.7560254794579));
#11646=CARTESIAN_POINT('Ctrl Pts',(-202.783049117812,93.6143808746666,11.7998225521413));
#11647=CARTESIAN_POINT('Ctrl Pts',(-202.487080653257,94.3105715849115,11.8436196248247));
#11648=CARTESIAN_POINT('Ctrl Pts',(-202.480886672631,95.0021035940924,11.887416697508));
#11649=CARTESIAN_POINT('Ctrl Pts',(-202.478890863588,94.9988537196689,11.612583302492));
#11650=CARTESIAN_POINT('Ctrl Pts',(-202.478525672062,94.9343767218714,11.6084912925661));
#11651=CARTESIAN_POINT('Ctrl Pts',(-202.480784445636,94.8699257260826,11.6043992826403));
#11652=CARTESIAN_POINT('Ctrl Pts',(-202.485749434321,94.8056838825638,11.6003072727144));
#11653=CARTESIAN_POINT('Ctrl Pts',(-202.550019236455,93.9740987906889,11.547337833113));
#11654=CARTESIAN_POINT('Ctrl Pts',(-203.067749801321,93.1775598219119,11.4943683935115));
#11655=CARTESIAN_POINT('Ctrl Pts',(-203.801616331267,92.7811959881444,11.4413989539101));
#11656=CARTESIAN_POINT('Ctrl Pts',(-204.535482861214,92.384832154377,11.3884295143086));
#11657=CARTESIAN_POINT('Ctrl Pts',(-205.485485356242,92.3886434556191,11.3354600747072));
#11658=CARTESIAN_POINT('Ctrl Pts',(-206.216147981621,92.7908828126805,11.2824906351058));
#11659=CARTESIAN_POINT('Ctrl Pts',(-206.946810607,93.1931221697419,11.2295211955043));
#11660=CARTESIAN_POINT('Ctrl Pts',(-207.45813336273,93.9937895826225,11.1765517559029));
#11661=CARTESIAN_POINT('Ctrl Pts',(-207.515728755059,94.825863583705,11.1235823163015));
#11662=CARTESIAN_POINT('Ctrl Pts',(-207.573324147388,95.6579375847875,11.0706128767));
#11663=CARTESIAN_POINT('Ctrl Pts',(-207.177192176316,96.5214181740719,11.0176434370986));
#11664=CARTESIAN_POINT('Ctrl Pts',(-206.508917523639,97.0204906749021,10.9646739974972));
#11665=CARTESIAN_POINT('Ctrl Pts',(-205.840642870963,97.5195631757323,10.9117045578957));
#11666=CARTESIAN_POINT('Ctrl Pts',(-204.900225536682,97.6542275881084,10.8587351182943));
#11667=CARTESIAN_POINT('Ctrl Pts',(-204.118747571406,97.3627544979554,10.8057656786929));
#11668=CARTESIAN_POINT('Ctrl Pts',(-203.33726960613,97.0712814078023,10.7527962390914));
#11669=CARTESIAN_POINT('Ctrl Pts',(-202.714731009859,96.3536708151202,10.69982679949));
#11670=CARTESIAN_POINT('Ctrl Pts',(-202.536499996132,95.5388714053017,10.6468573598885));
#11671=CARTESIAN_POINT('Ctrl Pts',(-202.498058333415,95.3631318219437,10.6354326740897));
#11672=CARTESIAN_POINT('Ctrl Pts',(-202.480285767457,95.1828710349325,10.6240079882908));
#11673=CARTESIAN_POINT('Ctrl Pts',(-202.481958520358,95.002283592634,10.612583302492));
#11674=CARTESIAN_POINT('Origin',(-205.,95.,9.));
#11675=CARTESIAN_POINT('',(-202.486537867015,94.9998805722871,9.61258330249198));
#11676=CARTESIAN_POINT('',(-202.482602635909,94.9976869505601,9.88741669750804));
#11677=CARTESIAN_POINT('',(-202.4825,95.,9.));
#11678=CARTESIAN_POINT('Ctrl Pts',(-202.482602635909,94.9976869505601,9.88741669750804));
#11679=CARTESIAN_POINT('Ctrl Pts',(-202.488423732856,95.6336264814084,9.92762245587553));
#11680=CARTESIAN_POINT('Ctrl Pts',(-202.733269733893,96.273556587542,9.96782821424303));
#11681=CARTESIAN_POINT('Ctrl Pts',(-203.168433611194,96.7333721687788,10.0080339726105));
#11682=CARTESIAN_POINT('Ctrl Pts',(-203.741744192846,97.3391603604975,10.061003412212));
#11683=CARTESIAN_POINT('Ctrl Pts',(-204.645389190247,97.6323240761667,10.1139728518134));
#11684=CARTESIAN_POINT('Ctrl Pts',(-205.465142786516,97.4784787068388,10.1669422914148));
#11685=CARTESIAN_POINT('Ctrl Pts',(-206.284896382785,97.3246333375108,10.2199117310163));
#11686=CARTESIAN_POINT('Ctrl Pts',(-207.020758577922,96.7237788831858,10.2728811706177));
#11687=CARTESIAN_POINT('Ctrl Pts',(-207.335414253965,95.9513436679131,10.3258506102191));
#11688=CARTESIAN_POINT('Ctrl Pts',(-207.650069930008,95.1789084526404,10.3788200498206));
#11689=CARTESIAN_POINT('Ctrl Pts',(-207.543519086958,94.2348924764201,10.431789489422));
#11690=CARTESIAN_POINT('Ctrl Pts',(-207.064604035821,93.552027387216,10.4847589290234));
#11691=CARTESIAN_POINT('Ctrl Pts',(-206.585688984684,92.869162298012,10.5377283686249));
#11692=CARTESIAN_POINT('Ctrl Pts',(-205.734409725459,92.4474480958241,10.5906978082263));
#11693=CARTESIAN_POINT('Ctrl Pts',(-204.900987913289,92.480196214229,10.6436672478278));
#11694=CARTESIAN_POINT('Ctrl Pts',(-204.067566101119,92.5129443326339,10.6966366874292));
#11695=CARTESIAN_POINT('Ctrl Pts',(-203.252001736004,93.0001547716316,10.7496061270306));
#11696=CARTESIAN_POINT('Ctrl Pts',(-202.828144965216,93.7184929887108,10.8025755666321));
#11697=CARTESIAN_POINT('Ctrl Pts',(-202.601847890061,94.1020136699879,10.8308559435907));
#11698=CARTESIAN_POINT('Ctrl Pts',(-202.487206701174,94.5514171099257,10.8591363205494));
#11699=CARTESIAN_POINT('Ctrl Pts',(-202.486464188569,95.0004666863557,10.887416697508));
#11700=CARTESIAN_POINT('Ctrl Pts',(-202.481958520358,95.002283592634,10.612583302492));
#11701=CARTESIAN_POINT('Ctrl Pts',(-202.488041322869,94.3455950007355,10.5710385486894));
#11702=CARTESIAN_POINT('Ctrl Pts',(-202.751257777578,93.684586908207,10.5294937948868));
#11703=CARTESIAN_POINT('Ctrl Pts',(-203.212761690374,93.2209570311217,10.4879490410842));
#11704=CARTESIAN_POINT('Ctrl Pts',(-203.801177829528,92.6298302937148,10.4349796014828));
#11705=CARTESIAN_POINT('Ctrl Pts',(-204.711933539022,92.3595650458559,10.3820101618814));
#11706=CARTESIAN_POINT('Ctrl Pts',(-205.527543491288,92.5340493668139,10.3290407222799));
#11707=CARTESIAN_POINT('Ctrl Pts',(-206.343153443554,92.7085336877719,10.2760712826785));
#11708=CARTESIAN_POINT('Ctrl Pts',(-207.063617638591,93.3277675775469,10.2231018430771));
#11709=CARTESIAN_POINT('Ctrl Pts',(-207.358679315634,94.1078976815906,10.1701324034756));
#11710=CARTESIAN_POINT('Ctrl Pts',(-207.653740992677,94.8880277856344,10.1171629638742));
#11711=CARTESIAN_POINT('Ctrl Pts',(-207.523400151727,95.8290541039469,10.0641935242728));
#11712=CARTESIAN_POINT('Ctrl Pts',(-207.027404305878,96.499615431042,10.0112240846713));
#11713=CARTESIAN_POINT('Ctrl Pts',(-206.531408460029,97.1701767581371,9.95825464506989));
#11714=CARTESIAN_POINT('Ctrl Pts',(-205.669757609282,97.5702730940147,9.90528520546845));
#11715=CARTESIAN_POINT('Ctrl Pts',(-204.837427688372,97.5165025142056,9.85231576586701));
#11716=CARTESIAN_POINT('Ctrl Pts',(-204.005097767462,97.4627319343966,9.79934632626558));
#11717=CARTESIAN_POINT('Ctrl Pts',(-203.202088776389,96.9550944389009,9.74637688666414));
#11718=CARTESIAN_POINT('Ctrl Pts',(-202.796495549129,96.226288218774,9.69340744706271));
#11719=CARTESIAN_POINT('Ctrl Pts',(-202.590202222992,95.8556019026464,9.66646606553913));
#11720=CARTESIAN_POINT('Ctrl Pts',(-202.48671858869,95.427700220413,9.63952468401556));
#11721=CARTESIAN_POINT('Ctrl Pts',(-202.486537867015,94.9998805722871,9.61258330249198));
#11722=CARTESIAN_POINT('Origin',(-205.,95.,9.));
#11723=CARTESIAN_POINT('',(-202.481519189143,94.9977697596226,8.61258330249198));
#11724=CARTESIAN_POINT('',(-202.478555055026,95.000793452331,8.88741669750803));
#11725=CARTESIAN_POINT('',(-202.4825,95.,9.));
#11726=CARTESIAN_POINT('Ctrl Pts',(-202.478555055026,95.000793452331,8.88741669750803));
#11727=CARTESIAN_POINT('Ctrl Pts',(-202.478376198151,95.0441568163808,8.89016971199881));
#11728=CARTESIAN_POINT('Ctrl Pts',(-202.479397808956,95.0875115778544,8.89292272648959));
#11729=CARTESIAN_POINT('Ctrl Pts',(-202.481646333745,95.1308026137449,8.89567574098038));
#11730=CARTESIAN_POINT('Ctrl Pts',(-202.524909127459,95.9637448007781,8.94864518058181));
#11731=CARTESIAN_POINT('Ctrl Pts',(-203.022372703672,96.7730959210315,9.00161462018325));
#11732=CARTESIAN_POINT('Ctrl Pts',(-203.746002539071,97.187853943956,9.05458405978468));
#11733=CARTESIAN_POINT('Ctrl Pts',(-204.46963237447,97.6026119668805,9.10755349938612));
#11734=CARTESIAN_POINT('Ctrl Pts',(-205.419428469055,97.6227768924762,9.16052293898755));
#11735=CARTESIAN_POINT('Ctrl Pts',(-206.160009600906,97.2391052315395,9.21349237858899));
#11736=CARTESIAN_POINT('Ctrl Pts',(-206.900590732757,96.8554335706029,9.26646181819042));
#11737=CARTESIAN_POINT('Ctrl Pts',(-207.431956901874,96.0679253231338,9.31943125779186));
#11738=CARTESIAN_POINT('Ctrl Pts',(-207.510532825818,95.2375698688638,9.3724006973933));
#11739=CARTESIAN_POINT('Ctrl Pts',(-207.589108749762,94.4072144145938,9.42537013699473));
#11740=CARTESIAN_POINT('Ctrl Pts',(-207.214894428534,93.5340117535228,9.47833957659617));
#11741=CARTESIAN_POINT('Ctrl Pts',(-206.559427615726,93.018233105683,9.53130901619761));
#11742=CARTESIAN_POINT('Ctrl Pts',(-205.903960802919,92.5024544578432,9.58427845579904));
#11743=CARTESIAN_POINT('Ctrl Pts',(-204.967241498532,92.3440998232346,9.63724789540047));
#11744=CARTESIAN_POINT('Ctrl Pts',(-204.178656596937,92.6157580814132,9.69021733500191));
#11745=CARTESIAN_POINT('Ctrl Pts',(-203.390071695343,92.8874163395918,9.74318677460335));
#11746=CARTESIAN_POINT('Ctrl Pts',(-202.74962119654,93.5890874905577,9.79615621420478));
#11747=CARTESIAN_POINT('Ctrl Pts',(-202.55088403009,94.3991293999248,9.84912565380622));
#11748=CARTESIAN_POINT('Ctrl Pts',(-202.502995703142,94.5943196227229,9.86188933504016));
#11749=CARTESIAN_POINT('Ctrl Pts',(-202.480754676092,94.7958022010768,9.8746530162741));
#11750=CARTESIAN_POINT('Ctrl Pts',(-202.482602635909,94.9976869505601,9.88741669750804));
#11751=CARTESIAN_POINT('Ctrl Pts',(-202.486537867015,94.9998805722871,9.61258330249198));
#11752=CARTESIAN_POINT('Ctrl Pts',(-202.486363271877,94.5865641787485,9.58655524441412));
#11753=CARTESIAN_POINT('Ctrl Pts',(-202.582606290008,94.1733243516167,9.56052718633626));
#11754=CARTESIAN_POINT('Ctrl Pts',(-202.775711662331,93.8118265903401,9.5344991282584));
#11755=CARTESIAN_POINT('Ctrl Pts',(-203.168698466242,93.0761461267913,9.48152968865697));
#11756=CARTESIAN_POINT('Ctrl Pts',(-203.96284953751,92.5547601444516,9.42856024905553));
#11757=CARTESIAN_POINT('Ctrl Pts',(-204.794130463097,92.486669063914,9.3755908094541));
#11758=CARTESIAN_POINT('Ctrl Pts',(-205.625411388685,92.4185779833763,9.32262136985266));
#11759=CARTESIAN_POINT('Ctrl Pts',(-206.493822168593,92.8037818046407,9.26965193025122));
#11760=CARTESIAN_POINT('Ctrl Pts',(-207.001288154334,93.4657052487113,9.21668249064978));
#11761=CARTESIAN_POINT('Ctrl Pts',(-207.508754140076,94.1276286927818,9.16371305104835));
#11762=CARTESIAN_POINT('Ctrl Pts',(-207.655275331652,95.0662717596585,9.11074361144692));
#11763=CARTESIAN_POINT('Ctrl Pts',(-207.373687233662,95.8513657129949,9.05777417184548));
#11764=CARTESIAN_POINT('Ctrl Pts',(-207.092099135672,96.6364596663312,9.00480473224405));
#11765=CARTESIAN_POINT('Ctrl Pts',(-206.382401748116,97.2680045061271,8.95183529264261));
#11766=CARTESIAN_POINT('Ctrl Pts',(-205.569916387379,97.4565036071433,8.89886585304117));
#11767=CARTESIAN_POINT('Ctrl Pts',(-204.757431026643,97.6450027081595,8.84589641343974));
#11768=CARTESIAN_POINT('Ctrl Pts',(-203.842157692726,97.3904560703959,8.79292697383831));
#11769=CARTESIAN_POINT('Ctrl Pts',(-203.243652566985,96.8095464500958,8.73995753423687));
#11770=CARTESIAN_POINT('Ctrl Pts',(-202.763916004669,96.3439137056573,8.69749945698858));
#11771=CARTESIAN_POINT('Ctrl Pts',(-202.487701496429,95.6685943106478,8.65504137974028));
#11772=CARTESIAN_POINT('Ctrl Pts',(-202.481519189143,94.9977697596226,8.61258330249198));
#11773=CARTESIAN_POINT('Origin',(-205.,95.,9.));
#11774=CARTESIAN_POINT('',(-202.47917661211,95.0013671579498,7.61258330249198));
#11775=CARTESIAN_POINT('',(-202.484976668263,95.0018590801224,7.88741669750804));
#11776=CARTESIAN_POINT('',(-202.4825,95.,9.));
#11777=CARTESIAN_POINT('Ctrl Pts',(-202.484976668263,95.0018590801224,7.88741669750804));
#11778=CARTESIAN_POINT('Ctrl Pts',(-202.48299671483,95.291524891365,7.90568640772354));
#11779=CARTESIAN_POINT('Ctrl Pts',(-202.529190133705,95.5805786424467,7.92395611793904));
#11780=CARTESIAN_POINT('Ctrl Pts',(-202.626312794037,95.8513657030603,7.94222582815454));
#11781=CARTESIAN_POINT('Ctrl Pts',(-202.907900888741,96.6364596472354,7.99519526775598));
#11782=CARTESIAN_POINT('Ctrl Pts',(-203.617598268015,97.2680044796619,8.04816470735741));
#11783=CARTESIAN_POINT('Ctrl Pts',(-204.430083619271,97.4565035784785,8.10113414695885));
#11784=CARTESIAN_POINT('Ctrl Pts',(-205.242568970527,97.6450026772951,8.15410358656028));
#11785=CARTESIAN_POINT('Ctrl Pts',(-206.157842293763,97.3904560425019,8.20707302616171));
#11786=CARTESIAN_POINT('Ctrl Pts',(-206.75634741252,96.8095464289804,8.26004246576315));
#11787=CARTESIAN_POINT('Ctrl Pts',(-207.354852531277,96.2286368154588,8.31301190536458));
#11788=CARTESIAN_POINT('Ctrl Pts',(-207.636589445553,95.321364223209,8.36598134496602));
#11789=CARTESIAN_POINT('Ctrl Pts',(-207.472411528303,94.5036173383193,8.41895078456746));
#11790=CARTESIAN_POINT('Ctrl Pts',(-207.308233611052,93.6858704534295,8.47192022416889));
#11791=CARTESIAN_POINT('Ctrl Pts',(-206.698140862275,92.9576492758997,8.52488966377033));
#11792=CARTESIAN_POINT('Ctrl Pts',(-205.92179638857,92.6527663239208,8.57785910337176));
#11793=CARTESIAN_POINT('Ctrl Pts',(-205.145451914865,92.3478833719418,8.6308285429732));
#11794=CARTESIAN_POINT('Ctrl Pts',(-204.202855716232,92.4663386455136,8.68379798257463));
#11795=CARTESIAN_POINT('Ctrl Pts',(-203.526088622524,92.9538329092061,8.73676742217607));
#11796=CARTESIAN_POINT('Ctrl Pts',(-202.884495576906,93.415990322401,8.78698384728672));
#11797=CARTESIAN_POINT('Ctrl Pts',(-202.481817498035,94.2098229977097,8.83720027239738));
#11798=CARTESIAN_POINT('Ctrl Pts',(-202.478555055026,95.000793452331,8.88741669750803));
#11799=CARTESIAN_POINT('Ctrl Pts',(-202.481519189143,94.9977697596226,8.61258330249198));
#11800=CARTESIAN_POINT('Ctrl Pts',(-202.479988632974,94.8316934700635,8.60207194013884));
#11801=CARTESIAN_POINT('Ctrl Pts',(-202.495008645671,94.6658926744072,8.5915605777857));
#11802=CARTESIAN_POINT('Ctrl Pts',(-202.527588442847,94.5036173325269,8.58104921543256));
#11803=CARTESIAN_POINT('Ctrl Pts',(-202.691766362013,93.6858704380949,8.52807977583112));
#11804=CARTESIAN_POINT('Ctrl Pts',(-203.30185911791,92.9576492520676,8.47511033622969));
#11805=CARTESIAN_POINT('Ctrl Pts',(-204.078203600674,92.652766296531,8.42214089662825));
#11806=CARTESIAN_POINT('Ctrl Pts',(-204.854548083438,92.3478833409944,8.36917145702682));
#11807=CARTESIAN_POINT('Ctrl Pts',(-205.79714429307,92.4663386159487,8.31620201742538));
#11808=CARTESIAN_POINT('Ctrl Pts',(-206.473911394675,92.9538328853297,8.26323257782395));
#11809=CARTESIAN_POINT('Ctrl Pts',(-207.150678496281,93.4413271547107,8.21026313822251));
#11810=CARTESIAN_POINT('Ctrl Pts',(-207.56161648986,94.2978604185185,8.15729369862107));
#11811=CARTESIAN_POINT('Ctrl Pts',(-207.518353695641,95.1308026152713,8.10432425901964));
#11812=CARTESIAN_POINT('Ctrl Pts',(-207.475090901422,95.963744812024,8.0513548194182));
#11813=CARTESIAN_POINT('Ctrl Pts',(-206.977627319405,96.7730959417216,7.99838537981677));
#11814=CARTESIAN_POINT('Ctrl Pts',(-206.253997475562,97.1878539694859,7.94541594021533));
#11815=CARTESIAN_POINT('Ctrl Pts',(-205.530367631719,97.6026119972502,7.8924465006139));
#11816=CARTESIAN_POINT('Ctrl Pts',(-204.580571526051,97.6227769230812,7.83947706101246));
#11817=CARTESIAN_POINT('Ctrl Pts',(-203.839990385558,97.2391052576674,7.78650762141103));
#11818=CARTESIAN_POINT('Ctrl Pts',(-203.099409245065,96.8554335922537,7.73353818180959));
#11819=CARTESIAN_POINT('Ctrl Pts',(-202.568043069748,96.0679253355952,7.68056874220816));
#11820=CARTESIAN_POINT('Ctrl Pts',(-202.489467144887,95.2375698716359,7.62759930260672));
#11821=CARTESIAN_POINT('Ctrl Pts',(-202.482042133373,95.1591056487688,7.62259396923514));
#11822=CARTESIAN_POINT('Ctrl Pts',(-202.478660201786,95.0802588322316,7.61758863586356));
#11823=CARTESIAN_POINT('Ctrl Pts',(-202.47917661211,95.0013671579498,7.61258330249198));
#11824=CARTESIAN_POINT('Origin',(-205.,95.,9.));
#11825=CARTESIAN_POINT('',(-202.485696042915,95.0014474120785,6.61258330249198));
#11826=CARTESIAN_POINT('',(-202.485291143957,94.9982947746438,6.88741669750803));
#11827=CARTESIAN_POINT('',(-202.4825,95.,9.));
#11828=CARTESIAN_POINT('Ctrl Pts',(-202.485291143957,94.9982947746438,6.88741669750803));
#11829=CARTESIAN_POINT('Ctrl Pts',(-202.488623019757,95.53414575907,6.92120310344825));
#11830=CARTESIAN_POINT('Ctrl Pts',(-202.656226186158,96.0718997890027,6.95498950938847));
#11831=CARTESIAN_POINT('Ctrl Pts',(-202.97259571778,96.499615413543,6.9887759153287));
#11832=CARTESIAN_POINT('Ctrl Pts',(-203.468591557841,97.1701767328134,7.04174535493013));
#11833=CARTESIAN_POINT('Ctrl Pts',(-204.330242398534,97.5702730640224,7.09471479453157));
#11834=CARTESIAN_POINT('Ctrl Pts',(-205.162572309731,97.5165024848408,7.147684234133));
#11835=CARTESIAN_POINT('Ctrl Pts',(-205.994902220929,97.4627319056592,7.20065367373444));
#11836=CARTESIAN_POINT('Ctrl Pts',(-206.797911202631,96.9550944160871,7.25362311333587));
#11837=CARTESIAN_POINT('Ctrl Pts',(-207.203504425158,96.2262882044646,7.30659255293731));
#11838=CARTESIAN_POINT('Ctrl Pts',(-207.609097647686,95.4974819928421,7.35956199253874));
#11839=CARTESIAN_POINT('Ctrl Pts',(-207.617275111038,94.5475070591692,7.41253143214018));
#11840=CARTESIAN_POINT('Ctrl Pts',(-207.224288311714,93.8118266042049,7.46550087174162));
#11841=CARTESIAN_POINT('Ctrl Pts',(-206.831301512389,93.0761461492407,7.51847031134305));
#11842=CARTESIAN_POINT('Ctrl Pts',(-206.037150450388,92.554760172985,7.57143975094449));
#11843=CARTESIAN_POINT('Ctrl Pts',(-205.205869534501,92.4866690932419,7.62440919054592));
#11844=CARTESIAN_POINT('Ctrl Pts',(-204.374588618613,92.4185780134987,7.67737863014736));
#11845=CARTESIAN_POINT('Ctrl Pts',(-203.506177848839,92.8037818302682,7.73034806974879));
#11846=CARTESIAN_POINT('Ctrl Pts',(-202.998711869018,93.4657052666148,7.78331750935023));
#11847=CARTESIAN_POINT('Ctrl Pts',(-202.666276179594,93.8993244305753,7.81801723873616));
#11848=CARTESIAN_POINT('Ctrl Pts',(-202.488737201272,94.4516957144252,7.8527169681221));
#11849=CARTESIAN_POINT('Ctrl Pts',(-202.484976668263,95.0018590801224,7.88741669750804));
#11850=CARTESIAN_POINT('Ctrl Pts',(-202.47917661211,95.0013671579498,7.61258330249198));
#11851=CARTESIAN_POINT('Ctrl Pts',(-202.484125165545,94.2453798210446,7.56461919626212));
#11852=CARTESIAN_POINT('Ctrl Pts',(-202.847043711761,93.4852733671239,7.51665509003227));
#11853=CARTESIAN_POINT('Ctrl Pts',(-203.440572366077,93.0182330825579,7.46869098380242));
#11854=CARTESIAN_POINT('Ctrl Pts',(-204.096039186533,92.5024544286996,7.41572154420098));
#11855=CARTESIAN_POINT('Ctrl Pts',(-205.03275850185,92.3440997922431,7.36275210459954));
#11856=CARTESIAN_POINT('Ctrl Pts',(-205.821343412647,92.6157580535917,7.3097826649981));
#11857=CARTESIAN_POINT('Ctrl Pts',(-206.609928323444,92.8874163149403,7.25681322539667));
#11858=CARTESIAN_POINT('Ctrl Pts',(-207.250378829719,93.589087474094,7.20384378579524));
#11859=CARTESIAN_POINT('Ctrl Pts',(-207.449115998488,94.3991293929133,7.15087434619381));
#11860=CARTESIAN_POINT('Ctrl Pts',(-207.647853167257,95.2091713117327,7.09790490659237));
#11861=CARTESIAN_POINT('Ctrl Pts',(-207.40487699852,96.1275839902179,7.04493546699093));
#11862=CARTESIAN_POINT('Ctrl Pts',(-206.831566410178,96.7333721890055,6.99196602738949));
#11863=CARTESIAN_POINT('Ctrl Pts',(-206.258255821837,97.3391603877931,6.93899658778806));
#11864=CARTESIAN_POINT('Ctrl Pts',(-205.354610813891,97.6323241068831,6.88602714818662));
#11865=CARTESIAN_POINT('Ctrl Pts',(-204.534857208056,97.4784787357599,6.83305770858519));
#11866=CARTESIAN_POINT('Ctrl Pts',(-203.715103602222,97.3246333646367,6.78008826898375));
#11867=CARTESIAN_POINT('Ctrl Pts',(-202.979241398498,96.7237789033003,6.72711882938231));
#11868=CARTESIAN_POINT('Ctrl Pts',(-202.664585718783,95.9513436790141,6.67414938978088));
#11869=CARTESIAN_POINT('Ctrl Pts',(-202.542678198843,95.6520779464127,6.65362736068458));
#11870=CARTESIAN_POINT('Ctrl Pts',(-202.483995110087,95.3270573987234,6.63310533158828));
#11871=CARTESIAN_POINT('Ctrl Pts',(-202.485696042915,95.0014474120785,6.61258330249198));
#11872=CARTESIAN_POINT('Origin',(-205.,95.,9.));
#11873=CARTESIAN_POINT('',(-202.484465795159,94.9979518675787,5.61258330249198));
#11874=CARTESIAN_POINT('',(-202.478772719,94.9989624714564,5.88741669750803));
#11875=CARTESIAN_POINT('',(-202.4825,95.,9.));
#11876=CARTESIAN_POINT('Ctrl Pts',(-202.478772719,94.9989624714564,5.88741669750803));
#11877=CARTESIAN_POINT('Ctrl Pts',(-202.482817100591,95.7757252592268,5.93671979917298));
#11878=CARTESIAN_POINT('Ctrl Pts',(-202.869063212578,96.5559620071741,5.98602290083791));
#11879=CARTESIAN_POINT('Ctrl Pts',(-203.491082493968,97.020490651325,6.03532600250285));
#11880=CARTESIAN_POINT('Ctrl Pts',(-204.159357138847,97.5195631463317,6.08829544210429));
#11881=CARTESIAN_POINT('Ctrl Pts',(-205.099774462154,97.6542275571366,6.14126488170573));
#11882=CARTESIAN_POINT('Ctrl Pts',(-205.881252418311,97.3627544703847,6.19423432130716));
#11883=CARTESIAN_POINT('Ctrl Pts',(-206.662730374467,97.0712813836329,6.2472037609086));
#11884=CARTESIAN_POINT('Ctrl Pts',(-207.285268963474,96.3536707993244,6.30017320051003));
#11885=CARTESIAN_POINT('Ctrl Pts',(-207.463499975122,95.5388713990138,6.35314264011147));
#11886=CARTESIAN_POINT('Ctrl Pts',(-207.64173098677,94.7240719987032,6.4061120797129));
#11887=CARTESIAN_POINT('Ctrl Pts',(-207.37565442106,93.8120837823904,6.45908151931434));
#11888=CARTESIAN_POINT('Ctrl Pts',(-206.787238288771,93.2209570518813,6.51205095891577));
#11889=CARTESIAN_POINT('Ctrl Pts',(-206.198822156483,92.6298303213723,6.56502039851721));
#11890=CARTESIAN_POINT('Ctrl Pts',(-205.288066457616,92.3595650766669,6.61798983811865));
#11891=CARTESIAN_POINT('Ctrl Pts',(-204.472456514868,92.5340493955888,6.67095927772008));
#11892=CARTESIAN_POINT('Ctrl Pts',(-203.65684657212,92.7085337145107,6.72392871732152));
#11893=CARTESIAN_POINT('Ctrl Pts',(-202.936382385489,93.3277675970599,6.77689815692295));
#11894=CARTESIAN_POINT('Ctrl Pts',(-202.641320711889,94.1078976920004,6.82986759652439));
#11895=CARTESIAN_POINT('Ctrl Pts',(-202.534463285052,94.3904240314138,6.8490506301856));
#11896=CARTESIAN_POINT('Ctrl Pts',(-202.483399392413,94.6940526634873,6.86823366384682));
#11897=CARTESIAN_POINT('Ctrl Pts',(-202.485291143957,94.9982947746438,6.88741669750803));
#11898=CARTESIAN_POINT('Ctrl Pts',(-202.485696042915,95.0014474120785,6.61258330249198));
#11899=CARTESIAN_POINT('Ctrl Pts',(-202.48838539032,94.4866249814282,6.58013589198684));
#11900=CARTESIAN_POINT('Ctrl Pts',(-202.642027659063,93.9703290230142,6.54768848148171));
#11901=CARTESIAN_POINT('Ctrl Pts',(-202.935395940087,93.5520273703197,6.51524107097657));
#11902=CARTESIAN_POINT('Ctrl Pts',(-203.414310996813,92.8691622731474,6.46227163137514));
#11903=CARTESIAN_POINT('Ctrl Pts',(-204.265590265972,92.4474480660385,6.4093021917737));
#11904=CARTESIAN_POINT('Ctrl Pts',(-205.099012087867,92.4801961848256,6.35633275217227));
#11905=CARTESIAN_POINT('Ctrl Pts',(-205.932433909762,92.5129443036126,6.30336331257083));
#11906=CARTESIAN_POINT('Ctrl Pts',(-206.747998284393,93.0001547482956,6.2503938729694));
#11907=CARTESIAN_POINT('Ctrl Pts',(-207.171855060127,93.718492973757,6.19742443336796));
#11908=CARTESIAN_POINT('Ctrl Pts',(-207.595711835862,94.4368311992184,6.14445499376652));
#11909=CARTESIAN_POINT('Ctrl Pts',(-207.627861012699,95.3862972054583,6.09148555416509));
#11910=CARTESIAN_POINT('Ctrl Pts',(-207.253565587638,96.1316610812089,6.03851611456365));
#11911=CARTESIAN_POINT('Ctrl Pts',(-206.879270162578,96.8770249569596,5.98554667496222));
#11912=CARTESIAN_POINT('Ctrl Pts',(-206.098530135621,97.4182867022209,5.93257723536078));
#11913=CARTESIAN_POINT('Ctrl Pts',(-205.269232372039,97.5073349577505,5.87960779575935));
#11914=CARTESIAN_POINT('Ctrl Pts',(-204.439934608457,97.59638321328,5.82663835615791));
#11915=CARTESIAN_POINT('Ctrl Pts',(-203.56207910825,97.2332179790778,5.77366891655647));
#11916=CARTESIAN_POINT('Ctrl Pts',(-203.038069926909,96.5843121689908,5.72069947695504));
#11917=CARTESIAN_POINT('Ctrl Pts',(-202.681550718245,96.1428172598422,5.68466075213402));
#11918=CARTESIAN_POINT('Ctrl Pts',(-202.488827307777,95.5690527658245,5.648622027313));
#11919=CARTESIAN_POINT('Ctrl Pts',(-202.484465795159,94.9979518675787,5.61258330249198));
#11920=CARTESIAN_POINT('Origin',(-205.,95.,9.));
#11921=CARTESIAN_POINT('',(-202.478335424994,94.9995851060564,4.61258330249197));
#11922=CARTESIAN_POINT('',(-202.482163844592,95.0022992344272,4.88741669750803));
#11923=CARTESIAN_POINT('',(-202.4825,95.,9.));
#11924=CARTESIAN_POINT('Ctrl Pts',(-202.482163844592,95.0022992344272,4.88741669750803));
#11925=CARTESIAN_POINT('Ctrl Pts',(-202.480430729047,95.189654321574,4.89926705529626));
#11926=CARTESIAN_POINT('Ctrl Pts',(-202.49956775128,95.3766586399814,4.91111741308448));
#11927=CARTESIAN_POINT('Ctrl Pts',(-202.540903035897,95.5586202943346,4.92296777087271));
#11928=CARTESIAN_POINT('Ctrl Pts',(-202.725665968888,96.3719634044993,4.97593721047414));
#11929=CARTESIAN_POINT('Ctrl Pts',(-203.353942368752,97.0845558622811,5.02890665007558));
#11930=CARTESIAN_POINT('Ctrl Pts',(-204.13773384485,97.369749267282,5.08187608967702));
#11931=CARTESIAN_POINT('Ctrl Pts',(-204.921525320947,97.6549426722829,5.13484552927845));
#11932=CARTESIAN_POINT('Ctrl Pts',(-205.860831873279,97.5127370245029,5.18781496887989));
#11933=CARTESIAN_POINT('Ctrl Pts',(-206.525080627473,97.0083185981828,5.24078440848132));
#11934=CARTESIAN_POINT('Ctrl Pts',(-207.189329381667,96.5039001718628,5.29375384808276));
#11935=CARTESIAN_POINT('Ctrl Pts',(-207.578520337724,95.6372689670026,5.34672328768419));
#11936=CARTESIAN_POINT('Ctrl Pts',(-207.51425053634,94.8056838848314,5.39969272728563));
#11937=CARTESIAN_POINT('Ctrl Pts',(-207.449980734956,93.9740988026602,5.45266216688706));
#11938=CARTESIAN_POINT('Ctrl Pts',(-206.932250176132,93.1775598431778,5.5056316064885));
#11939=CARTESIAN_POINT('Ctrl Pts',(-206.198383654749,92.7811960140355,5.55860104608994));
#11940=CARTESIAN_POINT('Ctrl Pts',(-205.464517133366,92.3848321848932,5.61157048569137));
#11941=CARTESIAN_POINT('Ctrl Pts',(-204.514514649423,92.3886434860908,5.66453992529281));
#11942=CARTESIAN_POINT('Ctrl Pts',(-203.78385203257,92.7908828384584,5.71750936489424));
#11943=CARTESIAN_POINT('Ctrl Pts',(-203.053189415717,93.1931221908261,5.77047880449568));
#11944=CARTESIAN_POINT('Ctrl Pts',(-202.541866665953,93.9937895943638,5.82344824409711));
#11945=CARTESIAN_POINT('Ctrl Pts',(-202.484271274297,94.8258635857369,5.87641768369855));
#11946=CARTESIAN_POINT('Ctrl Pts',(-202.480284746008,94.8834565008875,5.88008402163505));
#11947=CARTESIAN_POINT('Ctrl Pts',(-202.478471965718,94.9411998808629,5.88375035957154));
#11948=CARTESIAN_POINT('Ctrl Pts',(-202.478772719,94.9989624714564,5.88741669750803));
#11949=CARTESIAN_POINT('Ctrl Pts',(-202.484465795159,94.9979518675787,5.61258330249198));
#11950=CARTESIAN_POINT('Ctrl Pts',(-202.482416790193,94.7296530732386,5.59565258771156));
#11951=CARTESIAN_POINT('Ctrl Pts',(-202.521940158033,94.4619421472396,5.57872187293115));
#11952=CARTESIAN_POINT('Ctrl Pts',(-202.605583044702,94.2088096912299,5.56179115815073));
#11953=CARTESIAN_POINT('Ctrl Pts',(-202.867268206312,93.416859409528,5.5088217185493));
#11954=CARTESIAN_POINT('Ctrl Pts',(-203.56080139201,92.7676052320959,5.45585227894786));
#11955=CARTESIAN_POINT('Ctrl Pts',(-204.368270865209,92.5586616455789,5.40288283934642));
#11956=CARTESIAN_POINT('Ctrl Pts',(-205.175740338408,92.3497180590619,5.34991339974499));
#11957=CARTESIAN_POINT('Ctrl Pts',(-206.097146099108,92.5810850634599,5.29694396014356));
#11958=CARTESIAN_POINT('Ctrl Pts',(-206.710120895786,93.1467053169272,5.24397452054212));
#11959=CARTESIAN_POINT('Ctrl Pts',(-207.323095692464,93.7123255703945,5.19100508094069));
#11960=CARTESIAN_POINT('Ctrl Pts',(-207.62763952512,94.6121990729312,5.13803564133925));
#11961=CARTESIAN_POINT('Ctrl Pts',(-207.484151202775,95.4338288398249,5.08506620173782));
#11962=CARTESIAN_POINT('Ctrl Pts',(-207.34066288043,96.2554586067186,5.03209676213638));
#11963=CARTESIAN_POINT('Ctrl Pts',(-206.749142403085,96.9988446379694,4.97912732253494));
#11964=CARTESIAN_POINT('Ctrl Pts',(-205.980739451904,97.3232229311869,4.92615788293351));
#11965=CARTESIAN_POINT('Ctrl Pts',(-205.212336500722,97.6476012244043,4.87318844333207));
#11966=CARTESIAN_POINT('Ctrl Pts',(-204.267051075705,97.5529717795884,4.82021900373064));
#11967=CARTESIAN_POINT('Ctrl Pts',(-203.578196733049,97.082712205418,4.7672495641292));
#11968=CARTESIAN_POINT('Ctrl Pts',(-202.907731355322,96.6250062093864,4.71569414358346));
#11969=CARTESIAN_POINT('Ctrl Pts',(-202.48018894443,95.8114572920712,4.66413872303772));
#11970=CARTESIAN_POINT('Ctrl Pts',(-202.478335424994,94.9995851060564,4.61258330249197));
#11971=CARTESIAN_POINT('Origin',(-205.,95.,9.));
#11972=CARTESIAN_POINT('',(-202.483233810455,95.0022852208457,3.61258330249198));
#11973=CARTESIAN_POINT('',(-202.486523939152,94.9997695205866,3.88741669750803));
#11974=CARTESIAN_POINT('',(-202.4825,95.,9.));
#11975=CARTESIAN_POINT('Ctrl Pts',(-202.486523939152,94.9997695205866,3.88741669750803));
#11976=CARTESIAN_POINT('Ctrl Pts',(-202.486878327319,95.4343426674579,3.91478375102098));
#11977=CARTESIAN_POINT('Ctrl Pts',(-202.593838556984,95.8690792275426,3.94215080453392));
#11978=CARTESIAN_POINT('Ctrl Pts',(-202.80640580289,96.2439288606997,3.96951785804687));
#11979=CARTESIAN_POINT('Ctrl Pts',(-203.21783364944,96.9694572773319,4.0224872976483));
#11980=CARTESIAN_POINT('Ctrl Pts',(-204.024889883747,97.4706353696046,4.07545673724974));
#11981=CARTESIAN_POINT('Ctrl Pts',(-204.85762443817,97.517725900789,4.12842617685117));
#11982=CARTESIAN_POINT('Ctrl Pts',(-205.690358992592,97.5648164319734,4.18139561645261));
#11983=CARTESIAN_POINT('Ctrl Pts',(-206.54877186713,97.1578194020694,4.23436505605404));
#11984=CARTESIAN_POINT('Ctrl Pts',(-207.03937139724,96.4832999751306,4.28733449565548));
#11985=CARTESIAN_POINT('Ctrl Pts',(-207.529970927349,95.8087805481917,4.34030393525692));
#11986=CARTESIAN_POINT('Ctrl Pts',(-207.652757113031,94.866738724218,4.39327337485835));
#11987=CARTESIAN_POINT('Ctrl Pts',(-207.35144545295,94.0890012108126,4.44624281445979));
#11988=CARTESIAN_POINT('Ctrl Pts',(-207.050133792868,93.3112636974072,4.49921225406122));
#11989=CARTESIAN_POINT('Ctrl Pts',(-206.324724287023,92.69783049457,4.55218169366266));
#11990=CARTESIAN_POINT('Ctrl Pts',(-205.507740599016,92.529895954375,4.6051511332641));
#11991=CARTESIAN_POINT('Ctrl Pts',(-204.69075691101,92.3619614141801,4.65812057286553));
#11992=CARTESIAN_POINT('Ctrl Pts',(-203.782199040842,92.6395255366275,4.71109001246697));
#11993=CARTESIAN_POINT('Ctrl Pts',(-203.198544838816,93.2353544791249,4.7640594520684));
#11994=CARTESIAN_POINT('Ctrl Pts',(-202.745466137884,93.6978841796009,4.80517853388161));
#11995=CARTESIAN_POINT('Ctrl Pts',(-202.488177512802,94.3522033222036,4.84629761569482));
#11996=CARTESIAN_POINT('Ctrl Pts',(-202.482163844592,95.0022992344272,4.88741669750803));
#11997=CARTESIAN_POINT('Ctrl Pts',(-202.478335424994,94.9995851060564,4.61258330249197));
#11998=CARTESIAN_POINT('Ctrl Pts',(-202.478284588209,94.9773177531833,4.61116928343628));
#11999=CARTESIAN_POINT('Ctrl Pts',(-202.478553975643,94.9550516616304,4.60975526438059));
#12000=CARTESIAN_POINT('Ctrl Pts',(-202.479147358134,94.9327942077677,4.60834124532489));
#12001=CARTESIAN_POINT('Ctrl Pts',(-202.501375586168,94.0990254878127,4.55537180572346));
#12002=CARTESIAN_POINT('Ctrl Pts',(-202.978255302531,93.2773777514274,4.50240236612202));
#12003=CARTESIAN_POINT('Ctrl Pts',(-203.691187510233,92.8444897292865,4.44943292652059));
#12004=CARTESIAN_POINT('Ctrl Pts',(-204.404119717935,92.4116017071456,4.39646348691915));
#12005=CARTESIAN_POINT('Ctrl Pts',(-205.353104416976,92.367473399249,4.34349404731772));
#12006=CARTESIAN_POINT('Ctrl Pts',(-206.103132324622,92.7323329753115,4.29052460771628));
#12007=CARTESIAN_POINT('Ctrl Pts',(-206.853160232269,93.097192551374,4.23755516811485));
#12008=CARTESIAN_POINT('Ctrl Pts',(-207.40423134852,93.8710400113955,4.18458572851341));
#12009=CARTESIAN_POINT('Ctrl Pts',(-207.503737753283,94.6991480043073,4.13161628891197));
#12010=CARTESIAN_POINT('Ctrl Pts',(-207.603244158046,95.527255997219,4.07864684931054));
#12011=CARTESIAN_POINT('Ctrl Pts',(-207.251185851321,96.409624523021,4.0256774097091));
#12012=CARTESIAN_POINT('Ctrl Pts',(-206.608944393485,96.9417807804312,3.97270797010767));
#12013=CARTESIAN_POINT('Ctrl Pts',(-205.96670293565,97.4739370378414,3.91973853050623));
#12014=CARTESIAN_POINT('Ctrl Pts',(-205.034278326703,97.6558810268598,3.86676909090479));
#12015=CARTESIAN_POINT('Ctrl Pts',(-204.239088796595,97.4042106398603,3.81379965130336));
#12016=CARTESIAN_POINT('Ctrl Pts',(-203.443899266487,97.1525402528608,3.76083021170192));
#12017=CARTESIAN_POINT('Ctrl Pts',(-202.785944815216,96.4672554898434,3.70786077210049));
#12018=CARTESIAN_POINT('Ctrl Pts',(-202.566828086406,95.6624870561916,3.65489133249905));
#12019=CARTESIAN_POINT('Ctrl Pts',(-202.50849006353,95.4482240944041,3.64078865583003));
#12020=CARTESIAN_POINT('Ctrl Pts',(-202.481258909196,95.2254915716718,3.626685979161));
#12021=CARTESIAN_POINT('Ctrl Pts',(-202.483233810455,95.0022852208457,3.61258330249198));
#12022=CARTESIAN_POINT('Origin',(-205.,95.,9.));
#12023=CARTESIAN_POINT('',(-202.486304042859,94.9991964067408,2.61258330249198));
#12024=CARTESIAN_POINT('',(-202.481316067847,94.9978038198253,2.88741669750803));
#12025=CARTESIAN_POINT('',(-202.4825,95.,9.));
#12026=CARTESIAN_POINT('Ctrl Pts',(-202.481316067847,94.9978038198253,2.88741669750803));
#12027=CARTESIAN_POINT('Ctrl Pts',(-202.487520285317,95.6752130989754,2.9303004467457));
#12028=CARTESIAN_POINT('Ctrl Pts',(-202.769924095146,96.3571824133273,2.97318419598336));
#12029=CARTESIAN_POINT('Ctrl Pts',(-203.258228276972,96.823580482169,3.01606794522103));
#12030=CARTESIAN_POINT('Ctrl Pts',(-203.861375140903,97.3996692052147,3.06903738482246));
#12031=CARTESIAN_POINT('Ctrl Pts',(-204.778661392001,97.646863821374,3.1220068244239));
#12032=CARTESIAN_POINT('Ctrl Pts',(-205.589608139994,97.4518516989913,3.17497626402533));
#12033=CARTESIAN_POINT('Ctrl Pts',(-206.400554887986,97.2568395766086,3.22794570362677));
#12034=CARTESIAN_POINT('Ctrl Pts',(-207.105162132873,96.6196207156839,3.2809151432282));
#12035=CARTESIAN_POINT('Ctrl Pts',(-207.380441850704,95.8322926815315,3.33388458282964));
#12036=CARTESIAN_POINT('Ctrl Pts',(-207.655721568535,95.044964647379,3.38685402243108));
#12037=CARTESIAN_POINT('Ctrl Pts',(-207.501673759311,94.1075274399988,3.43982346203251));
#12038=CARTESIAN_POINT('Ctrl Pts',(-206.98891307815,93.4496970362421,3.49279290163395));
#12039=CARTESIAN_POINT('Ctrl Pts',(-206.47615239699,92.7918666324854,3.54576234123538));
#12040=CARTESIAN_POINT('Ctrl Pts',(-205.604678843892,92.4136430323522,3.59873178083682));
#12041=CARTESIAN_POINT('Ctrl Pts',(-204.773971025337,92.4884018205965,3.65170122043826));
#12042=CARTESIAN_POINT('Ctrl Pts',(-203.943263206782,92.5631606088408,3.70467066003969));
#12043=CARTESIAN_POINT('Ctrl Pts',(-203.153321122769,93.0909017854627,3.75764009964113));
#12044=CARTESIAN_POINT('Ctrl Pts',(-202.766249810158,93.8297117442694,3.81060953924256));
#12045=CARTESIAN_POINT('Ctrl Pts',(-202.579161759694,94.1868100627285,3.83621192533105));
#12046=CARTESIAN_POINT('Ctrl Pts',(-202.486192402449,94.5932182824481,3.86181431141954));
#12047=CARTESIAN_POINT('Ctrl Pts',(-202.486523939152,94.9997695205866,3.88741669750803));
#12048=CARTESIAN_POINT('Ctrl Pts',(-202.483233810455,95.0022852208457,3.61258330249198));
#12049=CARTESIAN_POINT('Ctrl Pts',(-202.488676608362,94.3871319044816,3.57371653955957));
#12050=CARTESIAN_POINT('Ctrl Pts',(-202.715952610492,93.7683796493997,3.53484977662716));
#12051=CARTESIAN_POINT('Ctrl Pts',(-203.125272191609,93.3134027435547,3.49598301369475));
#12052=CARTESIAN_POINT('Ctrl Pts',(-203.683112031973,92.6933389688557,3.44301357409331));
#12053=CARTESIAN_POINT('Ctrl Pts',(-204.57907071905,92.3774635237437,3.39004413449188));
#12054=CARTESIAN_POINT('Ctrl Pts',(-205.402445797958,92.5105719455655,3.33707469489044));
#12055=CARTESIAN_POINT('Ctrl Pts',(-206.225820876866,92.6436803673873,3.28410525528901));
#12056=CARTESIAN_POINT('Ctrl Pts',(-206.976612347604,93.2257726561428,3.23113581568757));
#12057=CARTESIAN_POINT('Ctrl Pts',(-207.310661595086,93.990020962638,3.17816637608613));
#12058=CARTESIAN_POINT('Ctrl Pts',(-207.644710842568,94.7542692691331,3.1251969364847));
#12059=CARTESIAN_POINT('Ctrl Pts',(-207.562017866793,95.7006735933678,3.07222749688326));
#12060=CARTESIAN_POINT('Ctrl Pts',(-207.10048866702,96.3954074757752,3.01925805728183));
#12061=CARTESIAN_POINT('Ctrl Pts',(-206.638959467246,97.0901413581826,2.96628861768039));
#12062=CARTESIAN_POINT('Ctrl Pts',(-205.798594043474,97.5332047987627,2.91331917807896));
#12063=CARTESIAN_POINT('Ctrl Pts',(-204.964611207011,97.5215000052282,2.86034973847752));
#12064=CARTESIAN_POINT('Ctrl Pts',(-204.130628370548,97.5097952116936,2.80738029887609));
#12065=CARTESIAN_POINT('Ctrl Pts',(-203.303028121394,97.0433221840444,2.75441085927465));
#12066=CARTESIAN_POINT('Ctrl Pts',(-202.86117779429,96.3359095247307,2.70144141967321));
#12067=CARTESIAN_POINT('Ctrl Pts',(-202.614104586054,95.940339566847,2.67182204727947));
#12068=CARTESIAN_POINT('Ctrl Pts',(-202.487647897893,95.4694324584975,2.64220267488572));
#12069=CARTESIAN_POINT('Ctrl Pts',(-202.486304042859,94.9991964067408,2.61258330249198));
#12070=CARTESIAN_POINT('Origin',(-205.,95.,9.));
#12071=CARTESIAN_POINT('',(-202.480282650156,94.9980775783256,1.61258330249198));
#12072=CARTESIAN_POINT('',(-202.479323465531,95.0014637551426,1.88741669750803));
#12073=CARTESIAN_POINT('',(-202.4825,95.,9.));
#12074=CARTESIAN_POINT('Ctrl Pts',(-202.479323465531,95.0014637551426,1.88741669750803));
#12075=CARTESIAN_POINT('Ctrl Pts',(-202.478731735526,95.0870778064218,1.89284770286898));
#12076=CARTESIAN_POINT('Ctrl Pts',(-202.482714810237,95.1726361517413,1.89827870822993));
#12077=CARTESIAN_POINT('Ctrl Pts',(-202.491454117109,95.25770588247,1.90370971359088));
#12078=CARTESIAN_POINT('Ctrl Pts',(-202.576689935662,96.087404191395,1.95667915319232));
#12079=CARTESIAN_POINT('Ctrl Pts',(-203.114357779528,96.8706235057184,2.00964859279375));
#12080=CARTESIAN_POINT('Ctrl Pts',(-203.857993540713,97.2483406348987,2.06261803239519));
#12081=CARTESIAN_POINT('Ctrl Pts',(-204.601629301898,97.626057764079,2.11558747199662));
#12082=CARTESIAN_POINT('Ctrl Pts',(-205.551232980402,97.5982727081163,2.16855691159806));
#12083=CARTESIAN_POINT('Ctrl Pts',(-206.271511640473,97.1777219009975,2.22152635119949));
#12084=CARTESIAN_POINT('Ctrl Pts',(-206.991790300543,96.7571710938786,2.27449579080093));
#12085=CARTESIAN_POINT('Ctrl Pts',(-207.482743942181,95.9438545356035,2.32746523040237));
#12086=CARTESIAN_POINT('Ctrl Pts',(-207.519322119212,95.1105920302357,2.3804346700038));
#12087=CARTESIAN_POINT('Ctrl Pts',(-207.555900296242,94.2773295248679,2.43340410960524));
#12088=CARTESIAN_POINT('Ctrl Pts',(-207.138103008664,93.4241210724073,2.48637354920667));
#12089=CARTESIAN_POINT('Ctrl Pts',(-206.457446217874,92.9420726405858,2.53934298880811));
#12090=CARTESIAN_POINT('Ctrl Pts',(-205.776789427083,92.4600242087642,2.59231242840954));
#12091=CARTESIAN_POINT('Ctrl Pts',(-204.833273133079,92.3491357975817,2.64528186801098));
#12092=CARTESIAN_POINT('Ctrl Pts',(-204.059399922816,92.6602380441338,2.69825130761242));
#12093=CARTESIAN_POINT('Ctrl Pts',(-203.285526712553,92.9713402906858,2.75122074721385));
#12094=CARTESIAN_POINT('Ctrl Pts',(-202.681296586031,93.7044331949723,2.80419018681529));
#12095=CARTESIAN_POINT('Ctrl Pts',(-202.523685261153,94.5234710620817,2.85715962641672));
#12096=CARTESIAN_POINT('Ctrl Pts',(-202.493675145273,94.6794206508639,2.86724531678049));
#12097=CARTESIAN_POINT('Ctrl Pts',(-202.479856917995,94.8384861211514,2.87733100714426));
#12098=CARTESIAN_POINT('Ctrl Pts',(-202.481316067847,94.9978038198253,2.88741669750803));
#12099=CARTESIAN_POINT('Ctrl Pts',(-202.486304042859,94.9991964067408,2.61258330249198));
#12100=CARTESIAN_POINT('Ctrl Pts',(-202.485244631304,94.628491610365,2.58923323528429));
#12101=CARTESIAN_POINT('Ctrl Pts',(-202.561939879356,94.2582038597523,2.5658831680766));
#12102=CARTESIAN_POINT('Ctrl Pts',(-202.718592679948,93.9255720971807,2.54253310086891));
#12103=CARTESIAN_POINT('Ctrl Pts',(-203.073958297766,93.1709996199226,2.48956366126747));
#12104=CARTESIAN_POINT('Ctrl Pts',(-203.840789938455,92.6102069563844,2.43659422166604));
#12105=CARTESIAN_POINT('Ctrl Pts',(-204.667576286735,92.5002582159558,2.3836247820646));
#12106=CARTESIAN_POINT('Ctrl Pts',(-205.494362635015,92.3903094755271,2.33065534246316));
#12107=CARTESIAN_POINT('Ctrl Pts',(-206.381103690885,92.731204658208,2.27768590286173));
#12108=CARTESIAN_POINT('Ctrl Pts',(-206.921322261313,93.3666795522678,2.22471646326029));
#12109=CARTESIAN_POINT('Ctrl Pts',(-207.46154083174,94.0021544463277,2.17174702365886));
#12110=CARTESIAN_POINT('Ctrl Pts',(-207.655236916725,94.9322090517666,2.11877758405742));
#12111=CARTESIAN_POINT('Ctrl Pts',(-207.413621413596,95.730511049215,2.06580814445599));
#12112=CARTESIAN_POINT('Ctrl Pts',(-207.172005910466,96.5288130466634,2.01283870485455));
#12113=CARTESIAN_POINT('Ctrl Pts',(-206.495078819221,97.1953624361213,1.95986926525312));
#12114=CARTESIAN_POINT('Ctrl Pts',(-205.693139528324,97.4246177066617,1.90689982565168));
#12115=CARTESIAN_POINT('Ctrl Pts',(-204.891200237426,97.6538729772021,1.85393038605024));
#12116=CARTESIAN_POINT('Ctrl Pts',(-203.964248746875,97.4458341288248,1.80096094644881));
#12117=CARTESIAN_POINT('Ctrl Pts',(-203.337194868197,96.8958629307826,1.74799150684737));
#12118=CARTESIAN_POINT('Ctrl Pts',(-202.80287268554,96.4272240770433,1.70285543872891));
#12119=CARTESIAN_POINT('Ctrl Pts',(-202.486306286811,95.7103079983322,1.65771937061044));
#12120=CARTESIAN_POINT('Ctrl Pts',(-202.480282650156,94.9980775783256,1.61258330249198));
#12121=CARTESIAN_POINT('Origin',(-205.,95.,9.));
#12122=CARTESIAN_POINT('',(-202.480223566112,95.0018649480296,0.612583302491977));
#12123=CARTESIAN_POINT('',(-202.485814060779,95.0013541851486,0.887416697508031));
#12124=CARTESIAN_POINT('',(-202.4825,95.,9.));
#12125=CARTESIAN_POINT('',(-206.913465996665,96.6359872033749,0.));
#12126=CARTESIAN_POINT('Ctrl Pts',(-202.480223566112,95.0018649480296,0.612583302491977));
#12127=CARTESIAN_POINT('Ctrl Pts',(-202.486186841973,94.2874533490054,0.567297187132291));
#12128=CARTESIAN_POINT('Ctrl Pts',(-202.805062530183,93.5684800237081,0.522011071772605));
#12129=CARTESIAN_POINT('Ctrl Pts',(-203.342523272204,93.0996259401887,0.476724956412919));
#12130=CARTESIAN_POINT('Ctrl Pts',(-203.971170575831,92.5512252248344,0.423755516811483));
#12131=CARTESIAN_POINT('Ctrl Pts',(-204.898866003489,92.3450148318929,0.370786077210047));
#12132=CARTESIAN_POINT('Ctrl Pts',(-205.70005254405,92.5769535947063,0.317816637608611));
#12133=CARTESIAN_POINT('Ctrl Pts',(-206.501239084611,92.8088923575197,0.264847198007175));
#12134=CARTESIAN_POINT('Ctrl Pts',(-207.175916738074,93.4789802760881,0.211877758405739));
#12135=CARTESIAN_POINT('Ctrl Pts',(-207.415094474449,94.2765455778558,0.158908318804303));
#12136=CARTESIAN_POINT('Ctrl Pts',(-207.654272210825,95.0741108796235,0.105938879202868));
#12137=CARTESIAN_POINT('Ctrl Pts',(-207.457950030113,95.9991535645904,0.0529694396014316));
#12138=CARTESIAN_POINT('Ctrl Pts',(-206.913465996665,96.6359872033749,-4.22296552189629E-15));
#12139=CARTESIAN_POINT('',(-203.082849217755,96.6387883341086,5.92619716121943E-15));
#12140=CARTESIAN_POINT('Origin',(-205.,95.,0.));
#12141=CARTESIAN_POINT('Ctrl Pts',(-203.082846187392,96.6387906377554,3.88578058618805E-15));
#12142=CARTESIAN_POINT('Ctrl Pts',(-203.61481511748,97.259358365042,0.0519060689145041));
#12143=CARTESIAN_POINT('Ctrl Pts',(-204.477409093976,97.5988875826691,0.103812137829004));
#12144=CARTESIAN_POINT('Ctrl Pts',(-205.289479051915,97.5049655305341,0.155718206743504));
#12145=CARTESIAN_POINT('Ctrl Pts',(-206.118185434207,97.4091193496953,0.20868764634494));
#12146=CARTESIAN_POINT('Ctrl Pts',(-206.894276478514,96.8618802331851,0.261657085946376));
#12147=CARTESIAN_POINT('Ctrl Pts',(-207.262506770502,96.113606687757,0.314626525547811));
#12148=CARTESIAN_POINT('Ctrl Pts',(-207.630737062491,95.365333142329,0.367595965149247));
#12149=CARTESIAN_POINT('Ctrl Pts',(-207.591106602161,94.4160251679831,0.420565404750683));
#12150=CARTESIAN_POINT('Ctrl Pts',(-207.161534857641,93.7010772548185,0.473534844352119));
#12151=CARTESIAN_POINT('Ctrl Pts',(-206.731963113121,92.9861293416538,0.526504283953555));
#12152=CARTESIAN_POINT('Ctrl Pts',(-205.912450084411,92.5055414896703,0.57947372355499));
#12153=CARTESIAN_POINT('Ctrl Pts',(-205.078775376487,92.4794977945143,0.632443163156426));
#12154=CARTESIAN_POINT('Ctrl Pts',(-204.245100668563,92.4534540993582,0.685412602757862));
#12155=CARTESIAN_POINT('Ctrl Pts',(-203.397264281424,92.8819545610296,0.738382042359298));
#12156=CARTESIAN_POINT('Ctrl Pts',(-202.923851916981,93.568632431485,0.791351481960734));
#12157=CARTESIAN_POINT('Ctrl Pts',(-202.637658839267,93.9837514015503,0.823373220476499));
#12158=CARTESIAN_POINT('Ctrl Pts',(-202.488302515099,94.4932237151927,0.855394958992265));
#12159=CARTESIAN_POINT('Ctrl Pts',(-202.485814060779,95.0013541851486,0.887416697508031));
#12160=CARTESIAN_POINT('Origin',(-205.,95.,-2.20842344717744));
#12161=CARTESIAN_POINT('',(-201.921316320141,95.0000395558662,16.2084234471775));
#12162=CARTESIAN_POINT('',(-201.931367598206,95.0007780422787,16.2915765528226));
#12163=CARTESIAN_POINT('',(-201.9265,95.0000000000003,-2.20842344717744));
#12164=CARTESIAN_POINT('',(-205.793799282533,92.0307770462543,17.));
#12165=CARTESIAN_POINT('Ctrl Pts',(-201.931367598206,95.0007780422787,16.2915765528226));
#12166=CARTESIAN_POINT('Ctrl Pts',(-201.930437927868,95.4711408136525,16.315839943476));
#12167=CARTESIAN_POINT('Ctrl Pts',(-202.253352122202,96.9670518748459,16.3930727737308));
#12168=CARTESIAN_POINT('Ctrl Pts',(-204.582352684019,98.6092822369636,16.5232750435871));
#12169=CARTESIAN_POINT('Ctrl Pts',(-207.810248235069,97.3070699809007,16.6821833623914));
#12170=CARTESIAN_POINT('Ctrl Pts',(-208.45646174186,93.8848225849406,16.8410916811957));
#12171=CARTESIAN_POINT('Ctrl Pts',(-206.782006578242,92.2949667869871,16.9470305603986));
#12172=CARTESIAN_POINT('Ctrl Pts',(-205.793799282533,92.0307770462543,17.));
#12173=CARTESIAN_POINT('',(-204.206200717467,92.0307770462543,17.));
#12174=CARTESIAN_POINT('Origin',(-205.,95.,17.));
#12175=CARTESIAN_POINT('Ctrl Pts',(-201.921316320141,95.0000395558662,16.2084234471775));
#12176=CARTESIAN_POINT('Ctrl Pts',(-201.921316128699,95.0014817728825,16.2084984707981));
#12177=CARTESIAN_POINT('Ctrl Pts',(-201.92196781021,96.0211820960645,16.2615429340201));
#12178=CARTESIAN_POINT('Ctrl Pts',(-203.036134055811,98.0574883854641,16.3675568368436));
#12179=CARTESIAN_POINT('Ctrl Pts',(-206.506730950831,98.3071022816236,16.5264651556479));
#12180=CARTESIAN_POINT('Ctrl Pts',(-208.595808661615,95.5240011654517,16.6853734744522));
#12181=CARTESIAN_POINT('Ctrl Pts',(-207.39670926564,92.2839837126632,16.8432184225696));
#12182=CARTESIAN_POINT('Ctrl Pts',(-205.168796249957,91.7689270082682,16.9480939310855));
#12183=CARTESIAN_POINT('Ctrl Pts',(-204.204429069408,92.0254062069443,17.));
#12184=CARTESIAN_POINT('Origin',(-205.,95.,-2.20842344717744));
#12185=CARTESIAN_POINT('',(-201.928214587435,95.0026730804178,15.2084234471775));
#12186=CARTESIAN_POINT('',(-201.926872884582,94.997179525272,15.2915765528226));
#12187=CARTESIAN_POINT('',(-201.9265,95.0000000000003,-2.20842344717744));
#12188=CARTESIAN_POINT('Ctrl Pts',(-201.926872884582,94.997179525272,15.2915765528226));
#12189=CARTESIAN_POINT('Ctrl Pts',(-201.933847634293,95.7655075466895,15.3313566392007));
#12190=CARTESIAN_POINT('Ctrl Pts',(-202.614657640989,97.5679292031576,15.4241061651802));
#12191=CARTESIAN_POINT('Ctrl Pts',(-205.64160296068,98.5768482546894,15.5698251307612));
#12192=CARTESIAN_POINT('Ctrl Pts',(-208.354341794396,96.3979033358336,15.7287334495655));
#12193=CARTESIAN_POINT('Ctrl Pts',(-207.991790848075,92.937312201061,15.8876417683699));
#12194=CARTESIAN_POINT('Ctrl Pts',(-204.886537417199,91.367902630111,16.0465500871741));
#12195=CARTESIAN_POINT('Ctrl Pts',(-202.343315689682,92.8593267432967,16.1811950153251));
#12196=CARTESIAN_POINT('Ctrl Pts',(-201.932467492388,94.4442912374762,16.2628705038745));
#12197=CARTESIAN_POINT('Ctrl Pts',(-201.931367598206,95.0007780422787,16.2915765528226));
#12198=CARTESIAN_POINT('Ctrl Pts',(-201.928214587436,95.0026730804178,15.2084234471775));
#12199=CARTESIAN_POINT('Ctrl Pts',(-201.925712666175,95.3041515486696,15.2240151665228));
#12200=CARTESIAN_POINT('Ctrl Pts',(-202.105035887535,96.626924896284,15.2925763254696));
#12201=CARTESIAN_POINT('Ctrl Pts',(-204.001156184096,98.4939765214113,15.4141069240178));
#12202=CARTESIAN_POINT('Ctrl Pts',(-207.396173510293,97.7320213368001,15.573015242822));
#12203=CARTESIAN_POINT('Ctrl Pts',(-208.594403628795,94.4653692735856,15.7319235616264));
#12204=CARTESIAN_POINT('Ctrl Pts',(-206.497329046882,91.688881880511,15.8908318804307));
#12205=CARTESIAN_POINT('Ctrl Pts',(-203.029149056991,91.947824442261,16.0496651756144));
#12206=CARTESIAN_POINT('Ctrl Pts',(-201.9214512941,93.9832234360713,16.1555290311966));
#12207=CARTESIAN_POINT('Ctrl Pts',(-201.921316320141,95.0000395558662,16.2084234471775));
#12208=CARTESIAN_POINT('Origin',(-205.,95.,-2.20842344717744));
#12209=CARTESIAN_POINT('',(-201.93080706636,94.9985876431865,14.2084234471775));
#12210=CARTESIAN_POINT('',(-201.921581992455,95.0008245399417,14.2915765528226));
#12211=CARTESIAN_POINT('',(-201.9265,95.0000000000003,-2.20842344717744));
#12212=CARTESIAN_POINT('Ctrl Pts',(-201.921581992455,95.0008245399417,14.2915765528226));
#12213=CARTESIAN_POINT('Ctrl Pts',(-201.92142212516,95.0455752780765,14.293903895324));
#12214=CARTESIAN_POINT('Ctrl Pts',(-201.942596684159,96.1086813249517,14.3492006774268));
#12215=CARTESIAN_POINT('Ctrl Pts',(-203.167697507449,98.1381902248446,14.4574668991311));
#12216=CARTESIAN_POINT('Ctrl Pts',(-206.645679958249,98.2399547180336,14.6163752179354));
#12217=CARTESIAN_POINT('Ctrl Pts',(-208.614921829979,95.3713653348348,14.7752835367397));
#12218=CARTESIAN_POINT('Ctrl Pts',(-207.270042916896,92.1623115429714,14.934191855544));
#12219=CARTESIAN_POINT('Ctrl Pts',(-203.844015795661,91.5548205083004,15.0931001743483));
#12220=CARTESIAN_POINT('Ctrl Pts',(-202.07012706505,93.4672252077733,15.2122284067745));
#12221=CARTESIAN_POINT('Ctrl Pts',(-201.924560359749,94.7424352401662,15.2783871995992));
#12222=CARTESIAN_POINT('Ctrl Pts',(-201.926872884582,94.997179525272,15.2915765528226));
#12223=CARTESIAN_POINT('Ctrl Pts',(-201.93080706636,94.9985876431865,14.2084234471775));
#12224=CARTESIAN_POINT('Ctrl Pts',(-201.933303438965,95.6013727123389,14.2395318622475));
#12225=CARTESIAN_POINT('Ctrl Pts',(-202.396531802648,97.2340830995271,14.323609716919));
#12226=CARTESIAN_POINT('Ctrl Pts',(-205.05099675704,98.6335890076928,14.4606570111919));
#12227=CARTESIAN_POINT('Ctrl Pts',(-208.082133999653,96.9251026119764,14.6195653299962));
#12228=CARTESIAN_POINT('Ctrl Pts',(-208.287605212672,93.451703526775,14.7784736488005));
#12229=CARTESIAN_POINT('Ctrl Pts',(-205.479036767596,91.3977656146854,14.9373819676048));
#12230=CARTESIAN_POINT('Ctrl Pts',(-202.549953847218,92.5238105299853,15.0806985670638));
#12231=CARTESIAN_POINT('Ctrl Pts',(-201.934212393764,94.2799447141626,15.1710457269214));
#12232=CARTESIAN_POINT('Ctrl Pts',(-201.928214587436,95.0026730804178,15.2084234471775));
#12233=CARTESIAN_POINT('Origin',(-205.,95.,-2.20842344717744));
#12234=CARTESIAN_POINT('',(-201.923038042999,94.9979784085099,13.2084234471775));
#12235=CARTESIAN_POINT('',(-201.92933278587,95.0023490188139,13.2915765528226));
#12236=CARTESIAN_POINT('',(-201.9265,95.0000000000003,-2.20842344717744));
#12237=CARTESIAN_POINT('Ctrl Pts',(-201.92933278587,95.0023490188139,13.2915765528226));
#12238=CARTESIAN_POINT('Ctrl Pts',(-201.926879380047,95.3476951209313,13.3094205910487));
#12239=CARTESIAN_POINT('Ctrl Pts',(-202.140117503338,96.7152487840609,13.3802340688762));
#12240=CARTESIAN_POINT('Ctrl Pts',(-204.150349511013,98.5332229241514,13.5040169863052));
#12241=CARTESIAN_POINT('Ctrl Pts',(-207.50996737673,97.6278572896369,13.6629253051096));
#12242=CARTESIAN_POINT('Ctrl Pts',(-208.568475210139,94.3133014680822,13.8218336239139));
#12243=CARTESIAN_POINT('Ctrl Pts',(-206.355444844063,91.6283031749969,13.9807419427182));
#12244=CARTESIAN_POINT('Ctrl Pts',(-202.95036918439,92.0284906781176,14.1373229190211));
#12245=CARTESIAN_POINT('Ctrl Pts',(-201.925060644632,94.0270653169006,14.2409344557225));
#12246=CARTESIAN_POINT('Ctrl Pts',(-201.921581992455,95.0008245399417,14.2915765528226));
#12247=CARTESIAN_POINT('Ctrl Pts',(-201.923038042999,94.9979784085099,13.2084234471775));
#12248=CARTESIAN_POINT('Ctrl Pts',(-201.929861215503,95.8956190998097,13.2550485579722));
#12249=CARTESIAN_POINT('Ctrl Pts',(-202.817787070614,97.8247938063492,13.3546431083684));
#12250=CARTESIAN_POINT('Ctrl Pts',(-206.096505488088,98.4645700435054,13.5072070983661));
#12251=CARTESIAN_POINT('Ctrl Pts',(-208.506304474045,95.9546720956722,13.6661154171704));
#12252=CARTESIAN_POINT('Ctrl Pts',(-207.701562707091,92.569541439018,13.8250237359747));
#12253=CARTESIAN_POINT('Ctrl Pts',(-204.420058445801,91.4126280298156,13.983932054779));
#12254=CARTESIAN_POINT('Ctrl Pts',(-202.208551988368,93.1272197714318,14.1117319585132));
#12255=CARTESIAN_POINT('Ctrl Pts',(-201.929052773747,94.5749884609644,14.1865624226461));
#12256=CARTESIAN_POINT('Ctrl Pts',(-201.93080706636,94.9985876431865,14.2084234471775));
#12257=CARTESIAN_POINT('Origin',(-205.,95.,-2.20842344717744));
#12258=CARTESIAN_POINT('',(-201.924530362794,95.0025681813082,12.2084234471775));
#12259=CARTESIAN_POINT('',(-201.930073873701,94.9980134193687,12.2915765528226));
#12260=CARTESIAN_POINT('',(-201.9265,95.0000000000003,-2.20842344717744));
#12261=CARTESIAN_POINT('Ctrl Pts',(-201.930073873701,94.9980134193687,12.2915765528226));
#12262=CARTESIAN_POINT('Ctrl Pts',(-201.933893697005,95.6440549307384,12.3249372867734));
#12263=CARTESIAN_POINT('Ctrl Pts',(-202.44913572334,97.3214395549061,12.4112674603257));
#12264=CARTESIAN_POINT('Ctrl Pts',(-205.205169260054,98.628150459449,12.5505670734794));
#12265=CARTESIAN_POINT('Ctrl Pts',(-208.161062843079,96.7925545691908,12.7094753922837));
#12266=CARTESIAN_POINT('Ctrl Pts',(-208.218929342183,93.3135646849756,12.868383711088));
#12267=CARTESIAN_POINT('Ctrl Pts',(-205.325717397541,91.3806798485012,13.0272920298923));
#12268=CARTESIAN_POINT('Ctrl Pts',(-202.492306008035,92.6103936505881,13.1683563104705));
#12269=CARTESIAN_POINT('Ctrl Pts',(-201.934162234404,94.3225465942424,13.2564511514472));
#12270=CARTESIAN_POINT('Ctrl Pts',(-201.92933278587,95.0023490188139,13.2915765528226));
#12271=CARTESIAN_POINT('Ctrl Pts',(-201.924530362794,95.0025681813082,12.2084234471775));
#12272=CARTESIAN_POINT('Ctrl Pts',(-201.922946673736,95.1793804353838,12.2175958140955));
#12273=CARTESIAN_POINT('Ctrl Pts',(-202.017340654133,96.3755745120124,12.279737620615));
#12274=CARTESIAN_POINT('Ctrl Pts',(-203.586712632674,98.3478633022839,12.3948488667359));
#12275=CARTESIAN_POINT('Ctrl Pts',(-207.048879131051,98.0012770914624,12.5537571855402));
#12276=CARTESIAN_POINT('Ctrl Pts',(-208.632656141981,94.9031535878521,12.7126655043445));
#12277=CARTESIAN_POINT('Ctrl Pts',(-206.886054603385,91.8938177924453,12.8715738231489));
#12278=CARTESIAN_POINT('Ctrl Pts',(-203.410339284457,91.7321951278126,13.0304821419532));
#12279=CARTESIAN_POINT('Ctrl Pts',(-201.98420370222,93.734861145707,13.1427653499627));
#12280=CARTESIAN_POINT('Ctrl Pts',(-201.922109606602,94.8758354773988,13.2020791183708));
#12281=CARTESIAN_POINT('Ctrl Pts',(-201.923038042999,94.9979784085099,13.2084234471775));
#12282=CARTESIAN_POINT('Origin',(-205.,95.,-2.20842344717744));
#12283=CARTESIAN_POINT('',(-201.931339695558,95.0005697559146,11.2084234471775));
#12284=CARTESIAN_POINT('',(-201.922093771296,94.9986005590476,11.2915765528226));
#12285=CARTESIAN_POINT('',(-201.9265,95.0000000000003,-2.20842344717744));
#12286=CARTESIAN_POINT('Ctrl Pts',(-201.922093771296,94.9986005590477,11.2915765528226));
#12287=CARTESIAN_POINT('Ctrl Pts',(-201.927419218831,95.9388438143246,11.3404539824981));
#12288=CARTESIAN_POINT('Ctrl Pts',(-202.890883267115,97.9074847478091,11.4423008517751));
#12289=CARTESIAN_POINT('Ctrl Pts',(-206.242562324195,98.4149098161,11.5971171606536));
#12290=CARTESIAN_POINT('Ctrl Pts',(-208.543663659863,95.8049956815827,11.7560254794579));
#12291=CARTESIAN_POINT('Ctrl Pts',(-207.595973758966,92.4570705034615,11.9149337982622));
#12292=CARTESIAN_POINT('Ctrl Pts',(-204.268324130509,91.4404746659679,12.0738421170665));
#12293=CARTESIAN_POINT('Ctrl Pts',(-202.169239397251,93.215538627184,12.19938970192));
#12294=CARTESIAN_POINT('Ctrl Pts',(-201.927828665579,94.6182844285985,12.271967847172));
#12295=CARTESIAN_POINT('Ctrl Pts',(-201.930073873701,94.9980134193687,12.2915765528226));
#12296=CARTESIAN_POINT('Ctrl Pts',(-201.931339695558,95.0005697559146,11.2084234471775));
#12297=CARTESIAN_POINT('Ctrl Pts',(-201.930548312084,95.4791749823821,11.2331125098202));
#12298=CARTESIAN_POINT('Ctrl Pts',(-202.261413021211,96.983573743505,11.3107710120644));
#12299=CARTESIAN_POINT('Ctrl Pts',(-204.612024672262,98.6131765827982,11.4413989539101));
#12300=CARTESIAN_POINT('Ctrl Pts',(-207.827224888828,97.2830613880067,11.6003072727144));
#12301=CARTESIAN_POINT('Ctrl Pts',(-208.450456926625,93.8598610299961,11.7592155915187));
#12302=CARTESIAN_POINT('Ctrl Pts',(-205.910348619136,91.4819273365871,11.918123910323));
#12303=CARTESIAN_POINT('Ctrl Pts',(-202.730434684324,92.2804106896555,12.0678598622093));
#12304=CARTESIAN_POINT('Ctrl Pts',(-201.932092308952,94.1583085466637,12.1646263744941));
#12305=CARTESIAN_POINT('Ctrl Pts',(-201.924530362794,95.0025681813082,12.2084234471775));
#12306=CARTESIAN_POINT('Origin',(-205.,95.,-2.20842344717744));
#12307=CARTESIAN_POINT('',(-201.926625303462,94.9971761042889,10.2084234471775));
#12308=CARTESIAN_POINT('',(-201.925838932402,95.0027879332515,10.2915765528226));
#12309=CARTESIAN_POINT('',(-201.9265,95.0000000000003,-2.20842344717744));
#12310=CARTESIAN_POINT('Ctrl Pts',(-201.925838932402,95.0027879332515,10.2915765528226));
#12311=CARTESIAN_POINT('Ctrl Pts',(-201.923796745295,95.2232588384768,10.3030012386214));
#12312=CARTESIAN_POINT('Ctrl Pts',(-202.046093760276,96.4636737691049,10.3673953640217));
#12313=CARTESIAN_POINT('Ctrl Pts',(-203.730077660409,98.4048300152887,10.4847589290234));
#12314=CARTESIAN_POINT('Ctrl Pts',(-207.174414514723,97.9116132469416,10.6436672478277));
#12315=CARTESIAN_POINT('Ctrl Pts',(-208.625272444921,94.7490619962975,10.802575566632));
#12316=CARTESIAN_POINT('Ctrl Pts',(-206.752521116536,91.8165679027658,10.9614838854363));
#12317=CARTESIAN_POINT('Ctrl Pts',(-203.273078016077,91.802608775416,11.1203922042406));
#12318=CARTESIAN_POINT('Ctrl Pts',(-201.96010201747,93.8226489641406,11.2304230933694));
#12319=CARTESIAN_POINT('Ctrl Pts',(-201.921647925753,94.91988355697,11.2874845428967));
#12320=CARTESIAN_POINT('Ctrl Pts',(-201.922093771296,94.9986005590477,11.2915765528226));
#12321=CARTESIAN_POINT('Ctrl Pts',(-201.926625303462,94.9971761042889,10.2084234471775));
#12322=CARTESIAN_POINT('Ctrl Pts',(-201.933732013081,95.7735654381765,10.248629205545));
#12323=CARTESIAN_POINT('Ctrl Pts',(-202.626469706802,97.5841063658898,10.3418044035139));
#12324=CARTESIAN_POINT('Ctrl Pts',(-205.670290596122,98.5715935365275,10.4879490410842));
#12325=CARTESIAN_POINT('Ctrl Pts',(-208.365431557495,96.3709268052048,10.6468573598885));
#12326=CARTESIAN_POINT('Ctrl Pts',(-207.975182481689,92.9134097014358,10.8057656786928));
#12327=CARTESIAN_POINT('Ctrl Pts',(-204.85731935967,91.3688552620022,10.9646739974972));
#12328=CARTESIAN_POINT('Ctrl Pts',(-202.334353177571,92.8760513997145,11.0988932536587));
#12329=CARTESIAN_POINT('Ctrl Pts',(-201.932246195058,94.4523457745213,11.1801430702188));
#12330=CARTESIAN_POINT('Ctrl Pts',(-201.931339695558,95.0005697559146,11.2084234471775));
#12331=CARTESIAN_POINT('Origin',(-205.,95.,-2.20842344717744));
#12332=CARTESIAN_POINT('',(-201.921683798062,95.0009686894698,9.20842344717747));
#12333=CARTESIAN_POINT('',(-201.931429646185,94.9998541961964,9.29157655282255));
#12334=CARTESIAN_POINT('',(-201.9265,95.0000000000003,-2.20842344717744));
#12335=CARTESIAN_POINT('Ctrl Pts',(-201.931429646185,94.9998541961964,9.29157655282255));
#12336=CARTESIAN_POINT('Ctrl Pts',(-201.931650280968,95.5221595342362,9.31851793434612));
#12337=CARTESIAN_POINT('Ctrl Pts',(-202.306382592467,97.0716662514915,9.39842875547113));
#12338=CARTESIAN_POINT('Ctrl Pts',(-204.765726364391,98.6263874648557,9.53130901619759));
#12339=CARTESIAN_POINT('Ctrl Pts',(-207.92157608408,97.1610098025081,9.69021733500189));
#12340=CARTESIAN_POINT('Ctrl Pts',(-208.398957503736,93.7144425063808,9.84912565380619));
#12341=CARTESIAN_POINT('Ctrl Pts',(-205.760212673412,91.4464599519933,10.0080339726105));
#12342=CARTESIAN_POINT('Ctrl Pts',(-202.664332879748,92.3651571515322,10.155517605616));
#12343=CARTESIAN_POINT('Ctrl Pts',(-201.933265146311,94.2010670247312,10.25003179902));
#12344=CARTESIAN_POINT('Ctrl Pts',(-201.925838932402,95.0027879332515,10.2915765528226));
#12345=CARTESIAN_POINT('Ctrl Pts',(-201.921683798062,95.0009686894698,9.20842344717747));
#12346=CARTESIAN_POINT('Ctrl Pts',(-201.921465439927,95.0539090268706,9.21117646166824));
#12347=CARTESIAN_POINT('Ctrl Pts',(-201.946710182927,96.1252365864707,9.26689891576045));
#12348=CARTESIAN_POINT('Ctrl Pts',(-203.192936169305,98.1527908565597,9.37559080945409));
#12349=CARTESIAN_POINT('Ctrl Pts',(-206.671623315332,98.2266461481009,9.5344991282584));
#12350=CARTESIAN_POINT('Ctrl Pts',(-208.617784889251,95.3423483146199,9.6934074470627));
#12351=CARTESIAN_POINT('Ctrl Pts',(-207.247201711938,92.1441893726518,9.85231576586701));
#12352=CARTESIAN_POINT('Ctrl Pts',(-203.81640912163,91.5642056950316,10.0112240846713));
#12353=CARTESIAN_POINT('Ctrl Pts',(-202.064207753662,93.4838999616225,10.1299266451081));
#12354=CARTESIAN_POINT('Ctrl Pts',(-201.924369214287,94.7507042959325,10.1956597659435));
#12355=CARTESIAN_POINT('Ctrl Pts',(-201.926625303462,94.9971761042889,10.2084234471775));
#12356=CARTESIAN_POINT('Origin',(-205.,95.,-2.20842344717744));
#12357=CARTESIAN_POINT('',(-201.92952365041,95.0022696654447,8.20842344717746));
#12358=CARTESIAN_POINT('',(-201.925302573121,94.9972772020656,8.29157655282255));
#12359=CARTESIAN_POINT('',(-201.9265,95.0000000000003,-2.20842344717744));
#12360=CARTESIAN_POINT('Ctrl Pts',(-201.925302573121,94.9972772020656,8.29157655282255));
#12361=CARTESIAN_POINT('Ctrl Pts',(-201.932850267835,95.8162560531386,8.33403463007084));
#12362=CARTESIAN_POINT('Ctrl Pts',(-202.690770542377,97.6693023124736,8.42946214692058));
#12363=CARTESIAN_POINT('Ctrl Pts',(-205.821273824104,98.5399264805142,8.57785910337175));
#12364=CARTESIAN_POINT('Ctrl Pts',(-208.420584553779,96.2268543075893,8.73676742217604));
#12365=CARTESIAN_POINT('Ctrl Pts',(-207.883941595716,92.7890158177634,8.89567574098036));
#12366=CARTESIAN_POINT('Ctrl Pts',(-204.70333321592,91.3781829144989,9.05458405978466));
#12367=CARTESIAN_POINT('Ctrl Pts',(-202.2878355418,92.9640356234163,9.1865509970654));
#12368=CARTESIAN_POINT('Ctrl Pts',(-201.931216491008,94.4952552148495,9.26554849474469));
#12369=CARTESIAN_POINT('Ctrl Pts',(-201.931429646185,94.9998541961964,9.29157655282255));
#12370=CARTESIAN_POINT('Ctrl Pts',(-201.92952365041,95.0022696654447,8.20842344717746));
#12371=CARTESIAN_POINT('Ctrl Pts',(-201.927106416298,95.3559093360916,8.22669315739296));
#12372=CARTESIAN_POINT('Ctrl Pts',(-202.147009294539,96.7319441344973,8.29793230720989));
#12373=CARTESIAN_POINT('Ctrl Pts',(-204.17872618548,98.5399264392071,8.42214089662825));
#12374=CARTESIAN_POINT('Ctrl Pts',(-207.530971538769,97.6076335907019,8.58104921543256));
#12375=CARTESIAN_POINT('Ctrl Pts',(-208.56285047346,94.2846914112228,8.73995753423687));
#12376=CARTESIAN_POINT('Ctrl Pts',(-206.328347915327,91.6175361510784,8.89886585304118));
#12377=CARTESIAN_POINT('Ctrl Pts',(-202.935840661412,92.0438696918247,9.0550211573547));
#12378=CARTESIAN_POINT('Ctrl Pts',(-201.925666764731,94.0353092287831,9.1582070220668));
#12379=CARTESIAN_POINT('Ctrl Pts',(-201.921683798062,95.0009686894698,9.20842344717747));
#12380=CARTESIAN_POINT('Origin',(-205.,95.,-2.20842344717744));
#12381=CARTESIAN_POINT('',(-201.929907579326,94.9979181687661,7.20842344717746));
#12382=CARTESIAN_POINT('',(-201.922442628529,95.0016691002816,7.29157655282255));
#12383=CARTESIAN_POINT('',(-201.9265,95.0000000000003,-2.20842344717744));
#12384=CARTESIAN_POINT('Ctrl Pts',(-201.922442628529,95.0016691002816,7.29157655282255));
#12385=CARTESIAN_POINT('Ctrl Pts',(-201.921812166908,95.0979843181188,7.29658188619413));
#12386=CARTESIAN_POINT('Ctrl Pts',(-201.96963492335,96.2129306162495,7.35455665916715));
#12387=CARTESIAN_POINT('Ctrl Pts',(-203.328376665162,98.2266461857523,7.46550087174159));
#12388=CARTESIAN_POINT('Ctrl Pts',(-206.807063851782,98.1527908933495,7.6244091905459));
#12389=CARTESIAN_POINT('Ctrl Pts',(-208.629055096267,95.1884921480159,7.78331750935021));
#12390=CARTESIAN_POINT('Ctrl Pts',(-207.123969189693,92.0513859081191,7.94222582815452));
#12391=CARTESIAN_POINT('Ctrl Pts',(-203.671652069173,91.6175361116086,8.10113414695882));
#12392=CARTESIAN_POINT('Ctrl Pts',(-202.034177280902,93.5720648629822,8.21758438851483));
#12393=CARTESIAN_POINT('Ctrl Pts',(-201.923433987467,94.794522296024,8.28106519046941));
#12394=CARTESIAN_POINT('Ctrl Pts',(-201.925302573121,94.9972772020656,8.29157655282255));
#12395=CARTESIAN_POINT('Ctrl Pts',(-201.929907579326,94.9979181687661,7.20842344717746));
#12396=CARTESIAN_POINT('Ctrl Pts',(-201.933975313296,95.6521139982133,7.24220985311768));
#12397=CARTESIAN_POINT('Ctrl Pts',(-202.459390605198,97.3379066754947,7.32896569865933));
#12398=CARTESIAN_POINT('Ctrl Pts',(-205.234273632875,98.6263874225397,7.46869098380241));
#12399=CARTESIAN_POINT('Ctrl Pts',(-208.175343867546,96.7671336101861,7.62759930260672));
#12400=CARTESIAN_POINT('Ctrl Pts',(-208.205294334613,93.2877914549009,7.78650762141103));
#12401=CARTESIAN_POINT('Ctrl Pts',(-205.296666780619,91.3781829567617,7.94541594021533));
#12402=CARTESIAN_POINT('Ctrl Pts',(-202.481733395465,92.6268122018764,8.08605454880414));
#12403=CARTESIAN_POINT('Ctrl Pts',(-201.934114712258,94.3306005077602,8.17372371779152));
#12404=CARTESIAN_POINT('Ctrl Pts',(-201.92952365041,95.0022696654447,8.20842344717746));
#12405=CARTESIAN_POINT('Origin',(-205.,95.,-2.20842344717744));
#12406=CARTESIAN_POINT('',(-201.921949534001,94.9987333291051,6.20842344717746));
#12407=CARTESIAN_POINT('',(-201.930401901847,95.0017670788574,6.29157655282255));
#12408=CARTESIAN_POINT('',(-201.9265,95.0000000000003,-2.20842344717744));
#12409=CARTESIAN_POINT('Ctrl Pts',(-201.930401901847,95.0017670788574,6.29157655282255));
#12410=CARTESIAN_POINT('Ctrl Pts',(-201.928325311163,95.3992893406063,6.31209858191885));
#12411=CARTESIAN_POINT('Ctrl Pts',(-202.184887900799,96.8202798707259,6.38559005061658));
#12412=CARTESIAN_POINT('Ctrl Pts',(-204.329709396056,98.5715935782041,6.51205095891576));
#12413=CARTESIAN_POINT('Ctrl Pts',(-207.639365322875,97.4978632616717,6.67095927772006));
#12414=CARTESIAN_POINT('Ctrl Pts',(-208.529280621322,94.13411982494,6.82986759652437));
#12415=CARTESIAN_POINT('Ctrl Pts',(-206.183590892181,91.5642056549396,6.98877591532867));
#12416=CARTESIAN_POINT('Ctrl Pts',(-202.86086221326,92.1259208703621,7.1426789007614));
#12417=CARTESIAN_POINT('Ctrl Pts',(-201.928484089891,94.0787189195554,7.2436124465927));
#12418=CARTESIAN_POINT('Ctrl Pts',(-201.922442628529,95.0016691002816,7.29157655282255));
#12419=CARTESIAN_POINT('Ctrl Pts',(-201.921949534001,94.9987333291051,6.20842344717746));
#12420=CARTESIAN_POINT('Ctrl Pts',(-201.926887133532,95.9470473025757,6.2577265488424));
#12421=CARTESIAN_POINT('Ctrl Pts',(-202.905053362444,97.9229927262678,6.35999909010877));
#12422=CARTESIAN_POINT('Ctrl Pts',(-206.269922324772,98.4048299755582,6.51524107097657));
#12423=CARTESIAN_POINT('Ctrl Pts',(-208.550008545203,95.7765366716391,6.67414938978089));
#12424=CARTESIAN_POINT('Ctrl Pts',(-207.575486609103,92.4363232263514,6.83305770858518));
#12425=CARTESIAN_POINT('Ctrl Pts',(-204.239787335459,91.4464599934592,6.9919660273895));
#12426=CARTESIAN_POINT('Ctrl Pts',(-202.162081150144,93.2322337929133,7.11708794025358));
#12427=CARTESIAN_POINT('Ctrl Pts',(-201.927598026844,94.6264829637453,7.18924041351624));
#12428=CARTESIAN_POINT('Ctrl Pts',(-201.929907579326,94.9979181687661,7.20842344717746));
#12429=CARTESIAN_POINT('Origin',(-205.,95.,-2.20842344717744));
#12430=CARTESIAN_POINT('',(-201.926089603319,95.0028070295978,5.20842344717746));
#12431=CARTESIAN_POINT('',(-201.928899948926,94.9974995292963,5.29157655282255));
#12432=CARTESIAN_POINT('',(-201.9265,95.0000000000003,-2.20842344717744));
#12433=CARTESIAN_POINT('Ctrl Pts',(-201.928899948926,94.9974995292963,5.29157655282255));
#12434=CARTESIAN_POINT('Ctrl Pts',(-201.934224719147,95.6947303578001,5.32761527764357));
#12435=CARTESIAN_POINT('Ctrl Pts',(-202.515335108225,97.4247770996434,5.41662344206602));
#12436=CARTESIAN_POINT('Ctrl Pts',(-205.387975332266,98.61317662496,5.55860104608992));
#12437=CARTESIAN_POINT('Ctrl Pts',(-208.247484138049,96.6307718892372,5.71750936489422));
#12438=CARTESIAN_POINT('Ctrl Pts',(-208.129735782527,93.1532937122619,5.87641768369853));
#12439=CARTESIAN_POINT('Ctrl Pts',(-205.142680641995,91.3688552196306,6.03532600250283));
#12440=CARTESIAN_POINT('Ctrl Pts',(-202.427470276955,92.7139399969898,6.17371229221084));
#12441=CARTESIAN_POINT('Ctrl Pts',(-201.933685202442,94.3732440438608,6.25912914231741));
#12442=CARTESIAN_POINT('Ctrl Pts',(-201.930401901847,95.0017670788574,6.29157655282255));
#12443=CARTESIAN_POINT('Ctrl Pts',(-201.926089603319,95.0028070295978,5.20842344717746));
#12444=CARTESIAN_POINT('Ctrl Pts',(-201.923973722235,95.2315402412545,5.22027380496568));
#12445=CARTESIAN_POINT('Ctrl Pts',(-202.0517688528,96.4803364748475,5.28509360235534));
#12446=CARTESIAN_POINT('Ctrl Pts',(-203.757437690304,98.4149097762516,5.40288283934642));
#12447=CARTESIAN_POINT('Ctrl Pts',(-207.197706236788,97.8940727651868,5.56179115815073));
#12448=CARTESIAN_POINT('Ctrl Pts',(-208.623142268693,94.7199821894518,5.72069947695504));
#12449=CARTESIAN_POINT('Ctrl Pts',(-206.726921963772,91.8026088127262,5.87960779575934));
#12450=CARTESIAN_POINT('Ctrl Pts',(-203.247478903914,91.8165679399129,6.03851611456365));
#12451=CARTESIAN_POINT('Ctrl Pts',(-201.955769853407,93.8392225784452,6.14812133170302));
#12452=CARTESIAN_POINT('Ctrl Pts',(-201.921582358147,94.9282136380667,6.20475710924096));
#12453=CARTESIAN_POINT('Ctrl Pts',(-201.921949534001,94.9987333291051,6.20842344717746));
#12454=CARTESIAN_POINT('Origin',(-205.,95.,-2.20842344717744));
#12455=CARTESIAN_POINT('',(-201.931412642297,94.9997186182815,4.20842344717746));
#12456=CARTESIAN_POINT('',(-201.921415661854,94.9994934750605,4.29157655282255));
#12457=CARTESIAN_POINT('',(-201.9265,95.0000000000003,-2.20842344717744));
#12458=CARTESIAN_POINT('Ctrl Pts',(-201.921415661854,94.9994934750605,4.29157655282255));
#12459=CARTESIAN_POINT('Ctrl Pts',(-201.923678538513,95.9906708985823,4.34313197336829));
#12460=CARTESIAN_POINT('Ctrl Pts',(-202.981928354028,98.0043611658593,4.44765683351546));
#12461=CARTESIAN_POINT('Ctrl Pts',(-206.413287383817,98.3478633413499,4.60515113326407));
#12462=CARTESIAN_POINT('Ctrl Pts',(-208.579767845133,95.6251658632375,4.76405945206838));
#12463=CARTESIAN_POINT('Ctrl Pts',(-207.464357156355,92.3293233090611,4.92296777087269));
#12464=CARTESIAN_POINT('Ctrl Pts',(-204.089651370241,91.481927295535,5.081876089677));
#12465=CARTESIAN_POINT('Ctrl Pts',(-202.125612719496,93.3205708167562,5.20474568366028));
#12466=CARTESIAN_POINT('Ctrl Pts',(-201.926398412972,94.6699458671693,5.27464583804213));
#12467=CARTESIAN_POINT('Ctrl Pts',(-201.928899948926,94.9974995292963,5.29157655282255));
#12468=CARTESIAN_POINT('Ctrl Pts',(-201.931412642297,94.9997186182815,4.20842344717746));
#12469=CARTESIAN_POINT('Ctrl Pts',(-201.931845298516,95.530268992426,4.2357905006904));
#12470=CARTESIAN_POINT('Ctrl Pts',(-202.31517360758,97.0882951016321,4.31612699380478));
#12471=CARTESIAN_POINT('Ctrl Pts',(-204.79483074234,98.6281504171124,4.44943292652058));
#12472=CARTESIAN_POINT('Ctrl Pts',(-207.938821173194,97.1374985345979,4.60834124532489));
#12473=CARTESIAN_POINT('Ctrl Pts',(-208.388533199045,93.6872118859588,4.76724956412919));
#12474=CARTESIAN_POINT('Ctrl Pts',(-205.731675860954,91.4404747075036,4.92615788293351));
#12475=CARTESIAN_POINT('Ctrl Pts',(-202.652180921301,92.3812593713882,5.07321584394959));
#12476=CARTESIAN_POINT('Ctrl Pts',(-201.933431414338,94.2091348205733,5.16730436536425));
#12477=CARTESIAN_POINT('Ctrl Pts',(-201.926089603319,95.0028070295978,5.20842344717746));
#12478=CARTESIAN_POINT('Origin',(-205.,95.,-2.20842344717744));
#12479=CARTESIAN_POINT('',(-201.925054591669,94.9973187846012,3.20842344717746));
#12480=CARTESIAN_POINT('',(-201.927395875445,95.0027899210604,3.29157655282255));
#12481=CARTESIAN_POINT('',(-201.9265,95.0000000000003,-2.20842344717744));
#12482=CARTESIAN_POINT('Ctrl Pts',(-201.927395875445,95.0027899210604,3.29157655282255));
#12483=CARTESIAN_POINT('Ctrl Pts',(-201.9249848093,95.2752922921681,3.30567922949157));
#12484=CARTESIAN_POINT('Ctrl Pts',(-202.083098781857,96.5685582167107,3.37275134576203));
#12485=CARTESIAN_POINT('Ctrl Pts',(-203.903494499117,98.4645700839332,3.49279290163393));
#12486=CARTESIAN_POINT('Ctrl Pts',(-207.318557500821,97.7981889317011,3.65170122043824));
#12487=CARTESIAN_POINT('Ctrl Pts',(-208.607992899891,94.5664594412711,3.81060953924254));
#12488=CARTESIAN_POINT('Ctrl Pts',(-206.589660734093,91.732195089681,3.96951785804685));
#12489=CARTESIAN_POINT('Ctrl Pts',(-203.113945374607,91.8938177561992,4.12842617685116));
#12490=CARTESIAN_POINT('Ctrl Pts',(-201.934002493894,93.9268197139999,4.23577907510972));
#12491=CARTESIAN_POINT('Ctrl Pts',(-201.921353597562,94.9723082877494,4.29016253376685));
#12492=CARTESIAN_POINT('Ctrl Pts',(-201.921415661854,94.9994934750605,4.29157655282255));
#12493=CARTESIAN_POINT('Ctrl Pts',(-201.925054591669,94.9973187846012,3.20842344717746));
#12494=CARTESIAN_POINT('Ctrl Pts',(-201.93262903552,95.8243366274881,3.25130719641512));
#12495=CARTESIAN_POINT('Ctrl Pts',(-202.703262931463,97.6853195581008,3.34716038525422));
#12496=CARTESIAN_POINT('Ctrl Pts',(-205.849650479072,98.5332228829228,3.49598301369474));
#12497=CARTESIAN_POINT('Ctrl Pts',(-208.430318245301,96.1993692554529,3.65489133249905));
#12498=CARTESIAN_POINT('Ctrl Pts',(-207.866108582956,92.7659473008752,3.81379965130336));
#12499=CARTESIAN_POINT('Ctrl Pts',(-204.67428260626,91.3806798907347,3.97270797010767));
#12500=CARTESIAN_POINT('Ctrl Pts',(-202.27933715358,92.9806849502469,4.10424923539903));
#12501=CARTESIAN_POINT('Ctrl Pts',(-201.93100788438,94.5033789041131,4.18282106108896));
#12502=CARTESIAN_POINT('Ctrl Pts',(-201.931412642297,94.9997186182815,4.20842344717746));
#12503=CARTESIAN_POINT('Origin',(-205.,95.,-2.20842344717744));
#12504=CARTESIAN_POINT('',(-201.922621915119,95.001787031353,2.20842344717746));
#12505=CARTESIAN_POINT('',(-201.931144181024,94.9990189299375,2.29157655282255));
#12506=CARTESIAN_POINT('',(-201.9265,95.0000000000003,-2.20842344717744));
#12507=CARTESIAN_POINT('Ctrl Pts',(-201.931144181024,94.9990189299375,2.29157655282255));
#12508=CARTESIAN_POINT('Ctrl Pts',(-201.932784831847,95.5731085049423,2.32119592521629));
#12509=CARTESIAN_POINT('Ctrl Pts',(-202.363262779912,97.1761484760171,2.40378473721147));
#12510=CARTESIAN_POINT('Ctrl Pts',(-204.949003242364,98.6335890500974,2.53934298880809));
#12511=CARTESIAN_POINT('Ctrl Pts',(-208.026893764665,97.0108417000006,2.69825130761239));
#12512=CARTESIAN_POINT('Ctrl Pts',(-208.329761920824,93.5445771233942,2.8571596264167));
#12513=CARTESIAN_POINT('Ctrl Pts',(-205.579941560967,91.4126279879542,3.01606794522101));
#12514=CARTESIAN_POINT('Ctrl Pts',(-202.589661751538,92.4668685231885,3.16087358735629));
#12515=CARTESIAN_POINT('Ctrl Pts',(-201.93404073716,94.2517775207246,3.25270978989014));
#12516=CARTESIAN_POINT('Ctrl Pts',(-201.927395875445,95.0027899210604,3.29157655282255));
#12517=CARTESIAN_POINT('Ctrl Pts',(-201.922621915119,95.001787031353,2.20842344717746));
#12518=CARTESIAN_POINT('Ctrl Pts',(-201.921899499162,95.1063092901838,2.2138544525384));
#12519=CARTESIAN_POINT('Ctrl Pts',(-201.974189435781,96.2295220789706,2.27225489750078));
#12520=CARTESIAN_POINT('Ctrl Pts',(-203.354320060973,98.2399546801978,2.3836247820646));
#12521=CARTESIAN_POINT('Ctrl Pts',(-206.832302471161,98.13819018824,2.54253310086891));
#12522=CARTESIAN_POINT('Ctrl Pts',(-208.630450654962,95.1593678146252,2.70144141967321));
#12523=CARTESIAN_POINT('Ctrl Pts',(-207.100242158396,92.0344389026441,2.86034973847752));
#12524=CARTESIAN_POINT('Ctrl Pts',(-203.644555171756,91.6283032143389,3.01925805728183));
#12525=CARTESIAN_POINT('Ctrl Pts',(-202.028743648494,93.5887151672915,3.13528262684847));
#12526=CARTESIAN_POINT('Ctrl Pts',(-201.923273182704,94.8028151314237,3.19833775681368));
#12527=CARTESIAN_POINT('Ctrl Pts',(-201.925054591669,94.9973187846012,3.20842344717746));
#12528=CARTESIAN_POINT('Origin',(-205.,95.,-2.20842344717744));
#12529=CARTESIAN_POINT('',(-201.930545984431,95.0016532623852,1.20842344717746));
#12530=CARTESIAN_POINT('',(-201.923792939525,94.9976530037673,1.29157655282255));
#12531=CARTESIAN_POINT('',(-201.9265,95.0000000000003,-2.20842344717744));
#12532=CARTESIAN_POINT('Ctrl Pts',(-201.923792939525,94.9976530037673,1.29157655282255));
#12533=CARTESIAN_POINT('Ctrl Pts',(-201.931146920561,95.8671823765141,1.33671262094101));
#12534=CARTESIAN_POINT('Ctrl Pts',(-202.771183541663,97.7695818819316,1.43481812866091));
#12535=CARTESIAN_POINT('Ctrl Pts',(-205.998843827582,98.4939765624303,1.58589307598225));
#12536=CARTESIAN_POINT('Ctrl Pts',(-208.478131313111,96.0526980537919,1.74480139478655));
#12537=CARTESIAN_POINT('Ctrl Pts',(-207.768707380001,92.6463153370295,1.90370971359086));
#12538=CARTESIAN_POINT('Ctrl Pts',(-204.520963226813,91.3977655726169,2.06261803239517));
#12539=CARTESIAN_POINT('Ctrl Pts',(-202.235891795972,93.0688641894186,2.19190697880573));
#12540=CARTESIAN_POINT('Ctrl Pts',(-201.929850794166,94.5464424883642,2.26822648561486));
#12541=CARTESIAN_POINT('Ctrl Pts',(-201.931144181024,94.9990189299375,2.29157655282255));
#12542=CARTESIAN_POINT('Ctrl Pts',(-201.930545984431,95.0016532623852,1.20842344717746));
#12543=CARTESIAN_POINT('Ctrl Pts',(-201.928558586322,95.4074704507228,1.22937114826312));
#12544=CARTESIAN_POINT('Ctrl Pts',(-202.192304342945,96.8369841963156,1.30328828895022));
#12545=CARTESIAN_POINT('Ctrl Pts',(-204.35839704753,98.5768482113765,1.43017486923876));
#12546=CARTESIAN_POINT('Ctrl Pts',(-207.659317996079,97.4766096293226,1.58908318804307));
#12547=CARTESIAN_POINT('Ctrl Pts',(-208.522221537982,94.105828029106,1.74799150684737));
#12548=CARTESIAN_POINT('Ctrl Pts',(-206.155984190728,91.5548205487187,1.90689982565168));
#12549=CARTESIAN_POINT('Ctrl Pts',(-202.847048345562,92.141549371385,2.06037713909504));
#12550=CARTESIAN_POINT('Ctrl Pts',(-201.928945334298,94.0868874505449,2.16088501293697));
#12551=CARTESIAN_POINT('Ctrl Pts',(-201.922621915119,95.001787031353,2.20842344717746));
#12552=CARTESIAN_POINT('Origin',(-205.,95.,-2.20842344717744));
#12553=CARTESIAN_POINT('',(-201.929615821727,94.9968993793473,0.208423447177457));
#12554=CARTESIAN_POINT('',(-201.923720806533,95.0022768293025,0.291576552822547));
#12555=CARTESIAN_POINT('',(-201.9265,95.0000000000003,-2.20842344717744));
#12556=CARTESIAN_POINT('',(-204.206200717467,92.0307770462543,0.));
#12557=CARTESIAN_POINT('Ctrl Pts',(-204.206200717467,92.0307770462543,-1.66533453693773E-15));
#12558=CARTESIAN_POINT('Ctrl Pts',(-203.217993421758,92.294966786987,0.0529694396014339));
#12559=CARTESIAN_POINT('Ctrl Pts',(-202.119889397913,93.3375904473839,0.12244392199392));
#12560=CARTESIAN_POINT('Ctrl Pts',(-201.927197935628,94.6776695912699,0.191918404386406));
#12561=CARTESIAN_POINT('Ctrl Pts',(-201.929615821727,94.9968993793473,0.208423447177457));
#12562=CARTESIAN_POINT('',(-205.795569479788,92.0254105888435,-2.77270672666423E-16));
#12563=CARTESIAN_POINT('Origin',(-205.,95.,0.));
#12564=CARTESIAN_POINT('Ctrl Pts',(-205.79557093555,92.025406175614,7.42000861794767E-16));
#12565=CARTESIAN_POINT('Ctrl Pts',(-204.831203783408,91.7689270056451,0.0519060689144966));
#12566=CARTESIAN_POINT('Ctrl Pts',(-202.766510651225,92.2462498650741,0.149098253188679));
#12567=CARTESIAN_POINT('Ctrl Pts',(-201.931001095851,94.1300845553796,0.246290437462861));
#12568=CARTESIAN_POINT('Ctrl Pts',(-201.923720806533,95.0022768293025,0.291576552822547));
#12569=CARTESIAN_POINT('Origin',(-205.,-95.,9.));
#12570=CARTESIAN_POINT('',(-202.486486965975,-94.9993627239001,16.612583302492));
#12571=CARTESIAN_POINT('',(-202.484598105996,-95.003732732209,16.887416697508));
#12572=CARTESIAN_POINT('',(-202.4825,-95.,9.));
#12573=CARTESIAN_POINT('',(-203.086534003335,-93.3640127966251,17.));
#12574=CARTESIAN_POINT('Ctrl Pts',(-202.484598105996,-95.003732732209,16.887416697508));
#12575=CARTESIAN_POINT('Ctrl Pts',(-202.489779960202,-94.411044798617,16.9249444650054));
#12576=CARTESIAN_POINT('Ctrl Pts',(-202.700778171916,-93.8151964396957,
16.9624722325027));
#12577=CARTESIAN_POINT('Ctrl Pts',(-203.086534003335,-93.3640127966251,
17.));
#12578=CARTESIAN_POINT('',(-202.4825,-95.,17.));
#12579=CARTESIAN_POINT('Origin',(-205.,-95.,17.));
#12580=CARTESIAN_POINT('',(-202.4825,-95.,18.));
#12581=CARTESIAN_POINT('',(-202.4825,-95.,9.));
#12582=CARTESIAN_POINT('Origin',(-205.,-95.,18.));
#12583=CARTESIAN_POINT('',(-206.91715084711,-93.3612115975349,17.));
#12584=CARTESIAN_POINT('Origin',(-205.,-95.,17.));
#12585=CARTESIAN_POINT('Ctrl Pts',(-206.917153877181,-93.3612092940951,
17.));
#12586=CARTESIAN_POINT('Ctrl Pts',(-206.38518496824,-92.7406416843865,16.9480939310855));
#12587=CARTESIAN_POINT('Ctrl Pts',(-205.522590942761,-92.4011122774809,
16.896187862171));
#12588=CARTESIAN_POINT('Ctrl Pts',(-204.710520941543,-92.4950342974083,
16.8442817932565));
#12589=CARTESIAN_POINT('Ctrl Pts',(-203.881814515085,-92.5908804453796,
16.7913123536551));
#12590=CARTESIAN_POINT('Ctrl Pts',(-203.10572343255,-93.1381196925948,16.7383429140536));
#12591=CARTESIAN_POINT('Ctrl Pts',(-202.737493126959,-93.8863932946479,
16.6853734744522));
#12592=CARTESIAN_POINT('Ctrl Pts',(-202.568820099224,-94.229150455359,16.6611100837988));
#12593=CARTESIAN_POINT('Ctrl Pts',(-202.48572547236,-94.614089163254,16.6368466931454));
#12594=CARTESIAN_POINT('Ctrl Pts',(-202.486486965975,-94.9993627239001,
16.612583302492));
#12595=CARTESIAN_POINT('Origin',(-205.,-95.,9.));
#12596=CARTESIAN_POINT('',(-202.482805352586,-95.0023102474081,15.612583302492));
#12597=CARTESIAN_POINT('',(-202.478253974141,-94.9999676034812,15.887416697508));
#12598=CARTESIAN_POINT('',(-202.4825,-95.,9.));
#12599=CARTESIAN_POINT('Ctrl Pts',(-202.478253974141,-94.9999676034812,
15.887416697508));
#12600=CARTESIAN_POINT('Ctrl Pts',(-202.478143102466,-94.1647321275155,
15.9404611607301));
#12601=CARTESIAN_POINT('Ctrl Pts',(-202.934422645956,-93.3296312577737,
15.9935056239521));
#12602=CARTESIAN_POINT('Ctrl Pts',(-203.637201829229,-92.8782275063029,
16.0465500871742));
#12603=CARTESIAN_POINT('Ctrl Pts',(-204.338987034326,-92.4274621992942,
16.0995195267756));
#12604=CARTESIAN_POINT('Ctrl Pts',(-205.28657426302,-92.3593094099306,16.152488966377));
#12605=CARTESIAN_POINT('Ctrl Pts',(-206.045561366399,-92.7051721137283,
16.2054584059785));
#12606=CARTESIAN_POINT('Ctrl Pts',(-206.804548469777,-93.051034817526,16.2584278455799));
#12607=CARTESIAN_POINT('Ctrl Pts',(-207.374935447839,-93.8109130144851,
16.3113972851814));
#12608=CARTESIAN_POINT('Ctrl Pts',(-207.495329357382,-94.6361476632023,
16.3643667247828));
#12609=CARTESIAN_POINT('Ctrl Pts',(-207.615723266924,-95.4613823119195,
16.4173361643842));
#12610=CARTESIAN_POINT('Ctrl Pts',(-207.286124107946,-96.3519734123947,
16.4703056039857));
#12611=CARTESIAN_POINT('Ctrl Pts',(-206.657476777652,-96.9003741267467,
16.5232750435871));
#12612=CARTESIAN_POINT('Ctrl Pts',(-206.028829447358,-97.4487748410986,
16.5762444831885));
#12613=CARTESIAN_POINT('Ctrl Pts',(-205.101133945748,-97.6549851693273,
16.62921392279));
#12614=CARTESIAN_POINT('Ctrl Pts',(-204.299947451515,-97.42304645291,16.6821833623914));
#12615=CARTESIAN_POINT('Ctrl Pts',(-203.498760957281,-97.1911077364927,
16.7351528019928));
#12616=CARTESIAN_POINT('Ctrl Pts',(-202.824083470424,-96.5210199754295,
16.7881222415943));
#12617=CARTESIAN_POINT('Ctrl Pts',(-202.584905723576,-95.7234546501587,
16.8410916811957));
#12618=CARTESIAN_POINT('Ctrl Pts',(-202.515180531668,-95.4909480892605,
16.8565333532998));
#12619=CARTESIAN_POINT('Ctrl Pts',(-202.482465911653,-95.2476079569009,
16.8719750254039));
#12620=CARTESIAN_POINT('Ctrl Pts',(-202.484598105996,-95.003732732209,16.887416697508));
#12621=CARTESIAN_POINT('Ctrl Pts',(-202.486486965975,-94.9993627239001,
16.612583302492));
#12622=CARTESIAN_POINT('Ctrl Pts',(-202.487387890058,-95.4551803731427,
16.5838772535439));
#12623=CARTESIAN_POINT('Ctrl Pts',(-202.605664630852,-95.9114667253842,
16.5551712045959));
#12624=CARTESIAN_POINT('Ctrl Pts',(-202.83846505618,-96.2989227836093,16.5264651556479));
#12625=CARTESIAN_POINT('Ctrl Pts',(-203.268036819641,-97.0138707136265,
16.4734957160464));
#12626=CARTESIAN_POINT('Ctrl Pts',(-204.087549875211,-97.4944586167699,
16.420526276445));
#12627=CARTESIAN_POINT('Ctrl Pts',(-204.921224617056,-97.5205023202695,
16.3675568368436));
#12628=CARTESIAN_POINT('Ctrl Pts',(-205.7548993589,-97.5465460237691,16.3145873972421));
#12629=CARTESIAN_POINT('Ctrl Pts',(-206.602735787018,-97.1180455276249,
16.2616179576407));
#12630=CARTESIAN_POINT('Ctrl Pts',(-207.076148172397,-96.4313676243484,
16.2086485180393));
#12631=CARTESIAN_POINT('Ctrl Pts',(-207.549560557776,-95.7446897210719,
16.1556790784378));
#12632=CARTESIAN_POINT('Ctrl Pts',(-207.648548900416,-94.7998344106631,
16.1027096388364));
#12633=CARTESIAN_POINT('Ctrl Pts',(-207.327709564386,-94.0299449024905,
16.049740199235));
#12634=CARTESIAN_POINT('Ctrl Pts',(-207.006870228356,-93.2600553943178,
15.9967707596335));
#12635=CARTESIAN_POINT('Ctrl Pts',(-206.266203213656,-92.6651316883815,
15.9438013200321));
#12636=CARTESIAN_POINT('Ctrl Pts',(-205.445239651077,-92.5178705169809,
15.8908318804307));
#12637=CARTESIAN_POINT('Ctrl Pts',(-204.624276088498,-92.3706093455804,
15.8378624408292));
#12638=CARTESIAN_POINT('Ctrl Pts',(-203.723015978041,-92.6710107087159,
15.7848930012278));
#12639=CARTESIAN_POINT('Ctrl Pts',(-203.154585383115,-93.2813785734586,
15.7319235616263));
#12640=CARTESIAN_POINT('Ctrl Pts',(-202.72769360672,-93.7397652689682,15.6921434752482));
#12641=CARTESIAN_POINT('Ctrl Pts',(-202.48851836135,-94.3729737086458,15.6523633888701));
#12642=CARTESIAN_POINT('Ctrl Pts',(-202.482805352586,-95.0023102474081,
15.612583302492));
#12643=CARTESIAN_POINT('Origin',(-205.,-95.,9.));
#12644=CARTESIAN_POINT('',(-202.478471589337,-94.9993246203416,14.612583302492));
#12645=CARTESIAN_POINT('',(-202.483904335665,-94.997810483196,14.887416697508));
#12646=CARTESIAN_POINT('',(-202.4825,-95.,9.));
#12647=CARTESIAN_POINT('Ctrl Pts',(-202.483904335665,-94.997810483196,14.887416697508));
#12648=CARTESIAN_POINT('Ctrl Pts',(-202.481855015029,-94.7508698395785,
14.9030084168534));
#12649=CARTESIAN_POINT('Ctrl Pts',(-202.515258260586,-94.5044716173505,
14.9186001361987));
#12650=CARTESIAN_POINT('Ctrl Pts',(-202.586378537099,-94.2694889359093,
14.934191855544));
#12651=CARTESIAN_POINT('Ctrl Pts',(-202.82799404516,-93.4711869221089,14.9871612951455));
#12652=CARTESIAN_POINT('Ctrl Pts',(-203.504921150218,-92.804637518854,15.0401307347469));
#12653=CARTESIAN_POINT('Ctrl Pts',(-204.30686045751,-92.5753822437128,15.0931001743483));
#12654=CARTESIAN_POINT('Ctrl Pts',(-205.108799764801,-92.3461269685716,
15.1460696139498));
#12655=CARTESIAN_POINT('Ctrl Pts',(-206.035751274325,-92.5541658215442,
15.1990390535512));
#12656=CARTESIAN_POINT('Ctrl Pts',(-206.662805165788,-93.1041370306651,
15.2520084931526));
#12657=CARTESIAN_POINT('Ctrl Pts',(-207.289859057251,-93.6541082397861,
15.3049779327541));
#12658=CARTESIAN_POINT('Ctrl Pts',(-207.617015330653,-94.5460118050555,
15.3579473723555));
#12659=CARTESIAN_POINT('Ctrl Pts',(-207.494308264464,-95.3709998251231,
15.410916811957));
#12660=CARTESIAN_POINT('Ctrl Pts',(-207.371601198275,-96.1959878451908,
15.4638862515584));
#12661=CARTESIAN_POINT('Ctrl Pts',(-206.799030792495,-96.9540603200567,
15.5168556911598));
#12662=CARTESIAN_POINT('Ctrl Pts',(-206.03905828976,-97.2977299359365,15.5698251307613));
#12663=CARTESIAN_POINT('Ctrl Pts',(-205.279085787025,-97.6413995518163,
15.6227945703627));
#12664=CARTESIAN_POINT('Ctrl Pts',(-204.331711187336,-97.57066630871,15.6757640099641));
#12665=CARTESIAN_POINT('Ctrl Pts',(-203.631209499739,-97.1179355866594,
15.7287334495656));
#12666=CARTESIAN_POINT('Ctrl Pts',(-202.9316999724,-96.6658460927997,15.7816278655464));
#12667=CARTESIAN_POINT('Ctrl Pts',(-202.478364532193,-95.8328404430598,
15.8345222815272));
#12668=CARTESIAN_POINT('Ctrl Pts',(-202.478253974141,-94.9999676034812,
15.887416697508));
#12669=CARTESIAN_POINT('Ctrl Pts',(-202.482805352586,-95.0023102474081,
15.612583302492));
#12670=CARTESIAN_POINT('Ctrl Pts',(-202.480911166388,-95.2109709784878,
15.5993939492687));
#12671=CARTESIAN_POINT('Ctrl Pts',(-202.504681444081,-95.4192060721596,
15.5862045960454));
#12672=CARTESIAN_POINT('Ctrl Pts',(-202.555783523722,-95.6205025079985,
15.573015242822));
#12673=CARTESIAN_POINT('Ctrl Pts',(-202.761013338649,-96.4289242114456,
15.5200458032206));
#12674=CARTESIAN_POINT('Ctrl Pts',(-203.407074047896,-97.1254332519901,
15.4670763636192));
#12675=CARTESIAN_POINT('Ctrl Pts',(-204.197813504076,-97.3907552453631,
15.4141069240177));
#12676=CARTESIAN_POINT('Ctrl Pts',(-204.988552960257,-97.6560772387361,
15.3611374844163));
#12677=CARTESIAN_POINT('Ctrl Pts',(-205.923971163369,-97.4902121849378,
15.3081680448149));
#12678=CARTESIAN_POINT('Ctrl Pts',(-206.575278375994,-96.9691909878947,
15.2551986052134));
#12679=CARTESIAN_POINT('Ctrl Pts',(-207.226585588618,-96.4481697908517,
15.202229165612));
#12680=CARTESIAN_POINT('Ctrl Pts',(-207.593781810755,-95.5719924505639,
15.1492597260106));
#12681=CARTESIAN_POINT('Ctrl Pts',(-207.508545988586,-94.7422941067118,
15.0962902864091));
#12682=CARTESIAN_POINT('Ctrl Pts',(-207.423310166418,-93.9125957628597,
15.0433208468077));
#12683=CARTESIAN_POINT('Ctrl Pts',(-206.885642299945,-93.1293764154432,
14.9903514072062));
#12684=CARTESIAN_POINT('Ctrl Pts',(-206.142006507432,-92.7516592703233,
14.9373819676048));
#12685=CARTESIAN_POINT('Ctrl Pts',(-205.398370714919,-92.3739421252033,
14.8844125280034));
#12686=CARTESIAN_POINT('Ctrl Pts',(-204.448766996366,-92.40172718238,14.8314430884019));
#12687=CARTESIAN_POINT('Ctrl Pts',(-203.728488305932,-92.8222780072335,
14.7784736488005));
#12688=CARTESIAN_POINT('Ctrl Pts',(-203.008209615498,-93.2428288320871,
14.7255042091991));
#12689=CARTESIAN_POINT('Ctrl Pts',(-202.517255953184,-94.0561454246176,
14.6725347695976));
#12690=CARTESIAN_POINT('Ctrl Pts',(-202.480677774616,-94.8894079650979,
14.6195653299962));
#12691=CARTESIAN_POINT('Ctrl Pts',(-202.479070622449,-94.9260194025585,
14.6172379874948));
#12692=CARTESIAN_POINT('Ctrl Pts',(-202.478340642232,-94.9626693456751,
14.6149106449934));
#12693=CARTESIAN_POINT('Ctrl Pts',(-202.478471589337,-94.9993246203416,
14.612583302492));
#12694=CARTESIAN_POINT('Origin',(-205.,-95.,9.));
#12695=CARTESIAN_POINT('',(-202.484820254705,-94.9980759215734,13.612583302492));
#12696=CARTESIAN_POINT('',(-202.486027831966,-95.0011568597348,13.887416697508));
#12697=CARTESIAN_POINT('',(-202.4825,-95.,9.));
#12698=CARTESIAN_POINT('Ctrl Pts',(-202.486027831966,-95.0011568597348,
13.887416697508));
#12699=CARTESIAN_POINT('Ctrl Pts',(-202.488072607706,-94.5074163488195,
13.9185251125781));
#12700=CARTESIAN_POINT('Ctrl Pts',(-202.628459862778,-94.012602672555,13.9496335276481));
#12701=CARTESIAN_POINT('Ctrl Pts',(-202.899511290069,-93.6045924957187,
13.9807419427182));
#12702=CARTESIAN_POINT('Ctrl Pts',(-203.361040499271,-92.9098585991177,
14.0337113823196));
#12703=CARTESIAN_POINT('Ctrl Pts',(-204.201405940211,-92.4667951494829,
14.0866808219211));
#12704=CARTESIAN_POINT('Ctrl Pts',(-205.035388793712,-92.4784999432582,
14.1396502615225));
#12705=CARTESIAN_POINT('Ctrl Pts',(-205.869371647213,-92.4902047370334,
14.1926197011239));
#12706=CARTESIAN_POINT('Ctrl Pts',(-206.696971913274,-92.9566777742187,
14.2455891407254));
#12707=CARTESIAN_POINT('Ctrl Pts',(-207.138822249404,-93.6640904479811,
14.2985585803268));
#12708=CARTESIAN_POINT('Ctrl Pts',(-207.580672585535,-94.3715031217434,
14.3515280199282));
#12709=CARTESIAN_POINT('Ctrl Pts',(-207.636772991736,-95.3198554320829,
14.4044974595297));
#12710=CARTESIAN_POINT('Ctrl Pts',(-207.281407366659,-96.0744279247623,
14.4574668991311));
#12711=CARTESIAN_POINT('Ctrl Pts',(-206.926041741582,-96.8290004174418,
14.5104363387325));
#12712=CARTESIAN_POINT('Ctrl Pts',(-206.159210085227,-97.3897930924613,
14.563405778334));
#12713=CARTESIAN_POINT('Ctrl Pts',(-205.332423720056,-97.4997418351244,
14.6163752179354));
#12714=CARTESIAN_POINT('Ctrl Pts',(-204.505637354885,-97.6096905777875,
14.6693446575369));
#12715=CARTESIAN_POINT('Ctrl Pts',(-203.618896280897,-97.2687953880943,
14.7223140971383));
#12716=CARTESIAN_POINT('Ctrl Pts',(-203.078677699436,-96.6333204810748,
14.7752835367397));
#12717=CARTESIAN_POINT('Ctrl Pts',(-202.697474138156,-96.1848995900276,
14.8126612569958));
#12718=CARTESIAN_POINT('Ctrl Pts',(-202.488817131473,-95.5897964016549,
14.8500389772519));
#12719=CARTESIAN_POINT('Ctrl Pts',(-202.483904335665,-94.997810483196,14.887416697508));
#12720=CARTESIAN_POINT('Ctrl Pts',(-202.478471589337,-94.9993246203416,
14.612583302492));
#12721=CARTESIAN_POINT('Ctrl Pts',(-202.481320949066,-95.7969296044664,
14.5619412053919));
#12722=CARTESIAN_POINT('Ctrl Pts',(-202.891803231304,-96.5970589773882,
14.5112991082919));
#12723=CARTESIAN_POINT('Ctrl Pts',(-203.5425537207,-97.0579274461484,14.4606570111919));
#12724=CARTESIAN_POINT('Ctrl Pts',(-204.223210540176,-97.5399758982885,
14.4076875715905));
#12725=CARTESIAN_POINT('Ctrl Pts',(-205.166726873948,-97.6508643141388,
14.354718131989));
#12726=CARTESIAN_POINT('Ctrl Pts',(-205.940600116827,-97.339762054474,14.3017486923876));
#12727=CARTESIAN_POINT('Ctrl Pts',(-206.714473359706,-97.0286597948092,
14.2487792527862));
#12728=CARTESIAN_POINT('Ctrl Pts',(-207.318703511691,-96.2955668596293,
14.1958098131847));
#12729=CARTESIAN_POINT('Ctrl Pts',(-207.476314843211,-95.4765289580023,
14.1428403735833));
#12730=CARTESIAN_POINT('Ctrl Pts',(-207.633926174731,-94.6574910563753,
14.0898709339818));
#12731=CARTESIAN_POINT('Ctrl Pts',(-207.344918685787,-93.7525081883012,
14.0369014943804));
#12732=CARTESIAN_POINT('Ctrl Pts',(-206.741771796435,-93.1764194409759,
13.983932054779));
#12733=CARTESIAN_POINT('Ctrl Pts',(-206.138624907084,-92.6003306936505,
13.9309626151775));
#12734=CARTESIAN_POINT('Ctrl Pts',(-205.221338617327,-92.353136067074,13.8779931755761));
#12735=CARTESIAN_POINT('Ctrl Pts',(-204.410391835157,-92.5481481976757,
13.8250237359747));
#12736=CARTESIAN_POINT('Ctrl Pts',(-203.599445052987,-92.7431603282774,
13.7720542963732));
#12737=CARTESIAN_POINT('Ctrl Pts',(-202.894837778405,-93.3803792160573,
13.7190848567718));
#12738=CARTESIAN_POINT('Ctrl Pts',(-202.619558048972,-94.1677072833915,
13.6661154171704));
#12739=CARTESIAN_POINT('Ctrl Pts',(-202.526823407038,-94.4329378056649,
13.6482713789442));
#12740=CARTESIAN_POINT('Ctrl Pts',(-202.482810673008,-94.7152033533037,
13.6304273407181));
#12741=CARTESIAN_POINT('Ctrl Pts',(-202.484820254705,-94.9980759215734,
13.612583302492));
#12742=CARTESIAN_POINT('Origin',(-205.,-95.,9.));
#12743=CARTESIAN_POINT('',(-202.485427278837,-95.0016272057563,12.612583302492));
#12744=CARTESIAN_POINT('',(-202.479664234459,-95.0016558831106,12.887416697508));
#12745=CARTESIAN_POINT('',(-202.4825,-95.,9.));
#12746=CARTESIAN_POINT('Ctrl Pts',(-202.479664234459,-95.0016558831106,
12.887416697508));
#12747=CARTESIAN_POINT('Ctrl Pts',(-202.48525308669,-94.2663994936904,12.9340418083028));
#12748=CARTESIAN_POINT('Ctrl Pts',(-202.825737534307,-93.526637293353,12.9806669190976));
#12749=CARTESIAN_POINT('Ctrl Pts',(-203.391055573645,-93.0582191799,13.0272920298924));
#12750=CARTESIAN_POINT('Ctrl Pts',(-204.033297044601,-92.5260629116183,
13.0802614694938));
#12751=CARTESIAN_POINT('Ctrl Pts',(-204.965721672596,-92.3441189188828,
13.1332309090952));
#12752=CARTESIAN_POINT('Ctrl Pts',(-205.76091121895,-92.5957893110237,13.1862003486967));
#12753=CARTESIAN_POINT('Ctrl Pts',(-206.556100765303,-92.8474597031646,
13.2391697882981));
#12754=CARTESIAN_POINT('Ctrl Pts',(-207.214055230015,-93.5327444801819,
13.2921392278995));
#12755=CARTESIAN_POINT('Ctrl Pts',(-207.433171963302,-94.3375129302743,
13.345108667501));
#12756=CARTESIAN_POINT('Ctrl Pts',(-207.652288696588,-95.1422813803668,
13.3980781071024));
#12757=CARTESIAN_POINT('Ctrl Pts',(-207.43256769845,-96.0665335035343,13.4510475467038));
#12758=CARTESIAN_POINT('Ctrl Pts',(-206.87472784669,-96.6865972909008,13.5040169863053));
#12759=CARTESIAN_POINT('Ctrl Pts',(-206.31688799493,-97.3066610782673,13.5569864259067));
#12760=CARTESIAN_POINT('Ctrl Pts',(-205.420929289549,-97.6225365298328,
13.6099558655081));
#12761=CARTESIAN_POINT('Ctrl Pts',(-204.59755419382,-97.4894281052916,13.6629253051096));
#12762=CARTESIAN_POINT('Ctrl Pts',(-203.774179098092,-97.3563196807503,
13.715894744711));
#12763=CARTESIAN_POINT('Ctrl Pts',(-203.023387612016,-96.7742273801023,
13.7688641843124));
#12764=CARTESIAN_POINT('Ctrl Pts',(-202.689338357709,-96.0099790579946,
13.8218336239139));
#12765=CARTESIAN_POINT('Ctrl Pts',(-202.551472845104,-95.6945660303437,
13.8436946484453));
#12766=CARTESIAN_POINT('Ctrl Pts',(-202.484590893038,-95.3481264304106,
13.8655556729767));
#12767=CARTESIAN_POINT('Ctrl Pts',(-202.486027831966,-95.0011568597348,
13.887416697508));
#12768=CARTESIAN_POINT('Ctrl Pts',(-202.484820254705,-94.9980759215734,
13.612583302492));
#12769=CARTESIAN_POINT('Ctrl Pts',(-202.48877605007,-95.5549012529596,13.5774579011167));
#12770=CARTESIAN_POINT('Ctrl Pts',(-202.671061992949,-96.1140787058531,
13.5423324997413));
#12771=CARTESIAN_POINT('Ctrl Pts',(-203.011086838027,-96.5503030290954,
13.507207098366));
#12772=CARTESIAN_POINT('Ctrl Pts',(-203.523847540798,-97.2081334605764,
13.4542376587646));
#12773=CARTESIAN_POINT('Ctrl Pts',(-204.395321130623,-97.5863570766498,
13.4012682191632));
#12774=CARTESIAN_POINT('Ctrl Pts',(-205.226028984189,-97.5115982852547,
13.3482987795617));
#12775=CARTESIAN_POINT('Ctrl Pts',(-206.056736837754,-97.4368394938597,
13.2953293399603));
#12776=CARTESIAN_POINT('Ctrl Pts',(-206.846678955059,-96.9090982949961,
13.2423599003589));
#12777=CARTESIAN_POINT('Ctrl Pts',(-207.233750283983,-96.1702883050523,
13.1893904607574));
#12778=CARTESIAN_POINT('Ctrl Pts',(-207.620821612906,-95.4314783151084,
13.136421021156));
#12779=CARTESIAN_POINT('Ctrl Pts',(-207.605022153448,-94.4815995340844,
13.0834515815546));
#12780=CARTESIAN_POINT('Ctrl Pts',(-207.193594289559,-93.7560710868749,
13.0304821419531));
#12781=CARTESIAN_POINT('Ctrl Pts',(-206.782166425669,-93.0305426396654,
12.9775127023517));
#12782=CARTESIAN_POINT('Ctrl Pts',(-205.975110157349,-92.5293645262705,
12.9245432627503));
#12783=CARTESIAN_POINT('Ctrl Pts',(-205.14237556783,-92.4822739931015,12.8715738231488));
#12784=CARTESIAN_POINT('Ctrl Pts',(-204.309640978312,-92.4351834599324,
12.8186043835474));
#12785=CARTESIAN_POINT('Ctrl Pts',(-203.451228067597,-92.8421805069893,
12.765634943946));
#12786=CARTESIAN_POINT('Ctrl Pts',(-202.960628516811,-93.5166999623558,
12.7126655043445));
#12787=CARTESIAN_POINT('Ctrl Pts',(-202.651643539561,-93.9415197124696,
12.6793047703937));
#12788=CARTESIAN_POINT('Ctrl Pts',(-202.488556091416,-94.4724553969259,
12.6459440364428));
#12789=CARTESIAN_POINT('Ctrl Pts',(-202.485427278837,-95.0016272057563,
12.612583302492));
#12790=CARTESIAN_POINT('Origin',(-205.,-95.,9.));
#12791=CARTESIAN_POINT('',(-202.478890786754,-95.001146280366,11.612583302492));
#12792=CARTESIAN_POINT('',(-202.480886591773,-94.9978964058402,11.887416697508));
#12793=CARTESIAN_POINT('',(-202.4825,-95.,9.));
#12794=CARTESIAN_POINT('Ctrl Pts',(-202.480886591773,-94.9978964058402,
11.887416697508));
#12795=CARTESIAN_POINT('Ctrl Pts',(-202.479589394008,-94.853069705361,11.8965890644261));
#12796=CARTESIAN_POINT('Ctrl Pts',(-202.491001823839,-94.7084473374192,
11.9057614313441));
#12797=CARTESIAN_POINT('Ctrl Pts',(-202.515848746476,-94.5661711513124,
11.9149337982622));
#12798=CARTESIAN_POINT('Ctrl Pts',(-202.659337071752,-93.7445413676335,
11.9679032378636));
#12799=CARTESIAN_POINT('Ctrl Pts',(-203.250857561182,-93.001155321196,12.0208726774651));
#12800=CARTESIAN_POINT('Ctrl Pts',(-204.019260528061,-92.6767770213518,
12.0738421170665));
#12801=CARTESIAN_POINT('Ctrl Pts',(-204.78766349494,-92.3523987215075,12.1268115566679));
#12802=CARTESIAN_POINT('Ctrl Pts',(-205.732948939268,-92.4470281682566,
12.1797809962694));
#12803=CARTESIAN_POINT('Ctrl Pts',(-206.421803295997,-92.9172877520339,
12.2327504358708));
#12804=CARTESIAN_POINT('Ctrl Pts',(-207.110657652725,-93.3875473358113,
12.2857198754723));
#12805=CARTESIAN_POINT('Ctrl Pts',(-207.543080921853,-94.2334370566169,
12.3386893150737));
#12806=CARTESIAN_POINT('Ctrl Pts',(-207.520852693365,-95.0672057936051,
12.3916587546751));
#12807=CARTESIAN_POINT('Ctrl Pts',(-207.498624464876,-95.9009745305933,
12.4446281942766));
#12808=CARTESIAN_POINT('Ctrl Pts',(-207.021744738771,-96.7226222837642,
12.497597633878));
#12809=CARTESIAN_POINT('Ctrl Pts',(-206.308812516505,-97.1555103147487,
12.5505670734794));
#12810=CARTESIAN_POINT('Ctrl Pts',(-205.595880294238,-97.5883983457332,
12.6035365130809));
#12811=CARTESIAN_POINT('Ctrl Pts',(-204.64689557581,-97.6325266545312,12.6565059526823));
#12812=CARTESIAN_POINT('Ctrl Pts',(-203.896867652842,-97.267667071015,12.7094753922837));
#12813=CARTESIAN_POINT('Ctrl Pts',(-203.146839729873,-96.9028074874987,
12.7624448318852));
#12814=CARTESIAN_POINT('Ctrl Pts',(-202.595768602363,-96.1289600116682,
12.8154142714866));
#12815=CARTESIAN_POINT('Ctrl Pts',(-202.496262195567,-95.3008520018389,
12.868383711088));
#12816=CARTESIAN_POINT('Ctrl Pts',(-202.484343976915,-95.2016667066702,
12.8747280398947));
#12817=CARTESIAN_POINT('Ctrl Pts',(-202.478903753345,-95.1017030081934,
12.8810723687014));
#12818=CARTESIAN_POINT('Ctrl Pts',(-202.479664234459,-95.0016558831106,
12.887416697508));
#12819=CARTESIAN_POINT('Ctrl Pts',(-202.485427278837,-95.0016272057563,
12.612583302492));
#12820=CARTESIAN_POINT('Ctrl Pts',(-202.483588231621,-95.3126627559102,
12.5929745968414));
#12821=CARTESIAN_POINT('Ctrl Pts',(-202.537012171023,-95.6230889170507,
12.5733658911908));
#12822=CARTESIAN_POINT('Ctrl Pts',(-202.648554447949,-95.9109988275815,
12.5537571855402));
#12823=CARTESIAN_POINT('Ctrl Pts',(-202.949866120729,-96.6887363737646,
12.5007877459388));
#12824=CARTESIAN_POINT('Ctrl Pts',(-203.675275657147,-97.302169602455,12.4478183063373));
#12825=CARTESIAN_POINT('Ctrl Pts',(-204.492259379585,-97.4701041497275,
12.3948488667359));
#12826=CARTESIAN_POINT('Ctrl Pts',(-205.309243102023,-97.638038697,12.3418794271345));
#12827=CARTESIAN_POINT('Ctrl Pts',(-206.217801010483,-97.3604745628546,
12.288909987533));
#12828=CARTESIAN_POINT('Ctrl Pts',(-206.801455237106,-96.764645595246,12.2359405479316));
#12829=CARTESIAN_POINT('Ctrl Pts',(-207.38510946373,-96.1688166276373,12.1829711083302));
#12830=CARTESIAN_POINT('Ctrl Pts',(-207.643860008518,-95.2547228265654,
12.1300016687287));
#12831=CARTESIAN_POINT('Ctrl Pts',(-207.459097067741,-94.4413796821223,
12.0770322291273));
#12832=CARTESIAN_POINT('Ctrl Pts',(-207.274334126964,-93.6280365376793,
12.0240627895259));
#12833=CARTESIAN_POINT('Ctrl Pts',(-206.646057700621,-92.9154440498653,
11.9710933499244));
#12834=CARTESIAN_POINT('Ctrl Pts',(-205.86226619149,-92.6302506328449,11.918123910323));
#12835=CARTESIAN_POINT('Ctrl Pts',(-205.07847468236,-92.3450572158246,11.8651544707215));
#12836=CARTESIAN_POINT('Ctrl Pts',(-204.139168090441,-92.4872628695979,
11.8121850311201));
#12837=CARTESIAN_POINT('Ctrl Pts',(-203.474919308252,-92.9916813171766,
11.7592155915187));
#12838=CARTESIAN_POINT('Ctrl Pts',(-202.861985258302,-93.457132290117,11.7103381618431));
#12839=CARTESIAN_POINT('Ctrl Pts',(-202.483252854292,-94.2309941842871,
11.6614607321675));
#12840=CARTESIAN_POINT('Ctrl Pts',(-202.478890786754,-95.001146280366,11.612583302492));
#12841=CARTESIAN_POINT('Origin',(-205.,-95.,9.));
#12842=CARTESIAN_POINT('',(-202.481958443618,-94.9977164072965,10.612583302492));
#12843=CARTESIAN_POINT('',(-202.486464107889,-94.9995333136293,10.887416697508));
#12844=CARTESIAN_POINT('',(-202.4825,-95.,9.));
#12845=CARTESIAN_POINT('Ctrl Pts',(-202.486464107889,-94.9995333136293,
10.887416697508));
#12846=CARTESIAN_POINT('Ctrl Pts',(-202.485815886657,-94.6075083595682,
10.9121057601508));
#12847=CARTESIAN_POINT('Ctrl Pts',(-202.571975216773,-94.2157531015706,
10.9367948227936));
#12848=CARTESIAN_POINT('Ctrl Pts',(-202.746434366323,-93.8683388956723,
10.9614838854364));
#12849=CARTESIAN_POINT('Ctrl Pts',(-203.12072979903,-93.1229750046945,11.0144533250378));
#12850=CARTESIAN_POINT('Ctrl Pts',(-203.901469841937,-92.5817132483756,
11.0674227646392));
#12851=CARTESIAN_POINT('Ctrl Pts',(-204.730767622461,-92.4926649910269,
11.1203922042407));
#12852=CARTESIAN_POINT('Ctrl Pts',(-205.560065402984,-92.4036167336781,
11.1733616438421));
#12853=CARTESIAN_POINT('Ctrl Pts',(-206.437920921125,-92.7667819752994,
11.2263310834435));
#12854=CARTESIAN_POINT('Ctrl Pts',(-206.961930113172,-93.415687798643,11.279300523045));
#12855=CARTESIAN_POINT('Ctrl Pts',(-207.485939305218,-94.0645936219866,
11.3322699626464));
#12856=CARTESIAN_POINT('Ctrl Pts',(-207.656102171171,-94.9992400270525,
11.3852394022478));
#12857=CARTESIAN_POINT('Ctrl Pts',(-207.394417004214,-95.7911903249334,
11.4382088418493));
#12858=CARTESIAN_POINT('Ctrl Pts',(-207.132731837258,-96.5831406228142,
11.4911782814507));
#12859=CARTESIAN_POINT('Ctrl Pts',(-206.439198637392,-97.2323948135099,
11.5441477210522));
#12860=CARTESIAN_POINT('Ctrl Pts',(-205.631729147697,-97.4413384042955,
11.5971171606536));
#12861=CARTESIAN_POINT('Ctrl Pts',(-204.824259658002,-97.650281995081,11.650086600255));
#12862=CARTESIAN_POINT('Ctrl Pts',(-203.902853878478,-97.4189149859564,
11.7030560398565));
#12863=CARTESIAN_POINT('Ctrl Pts',(-203.289879069277,-96.853294720934,11.7560254794579));
#12864=CARTESIAN_POINT('Ctrl Pts',(-202.783049046652,-96.3856191698091,
11.7998225521413));
#12865=CARTESIAN_POINT('Ctrl Pts',(-202.487080572597,-95.6894284372179,
11.8436196248246));
#12866=CARTESIAN_POINT('Ctrl Pts',(-202.480886591773,-94.9978964058402,
11.887416697508));
#12867=CARTESIAN_POINT('Ctrl Pts',(-202.478890786754,-95.001146280366,11.612583302492));
#12868=CARTESIAN_POINT('Ctrl Pts',(-202.478525595217,-95.0656232801284,
11.6084912925661));
#12869=CARTESIAN_POINT('Ctrl Pts',(-202.480784368861,-95.1300742778814,
11.6043992826402));
#12870=CARTESIAN_POINT('Ctrl Pts',(-202.485749357697,-95.1943161233581,
11.6003072727144));
#12871=CARTESIAN_POINT('Ctrl Pts',(-202.550019161789,-96.0259012405764,
11.5473378331129));
#12872=CARTESIAN_POINT('Ctrl Pts',(-203.067749742433,-96.8224402336289,
11.4943683935115));
#12873=CARTESIAN_POINT('Ctrl Pts',(-203.801616294745,-97.218804079476,11.4413989539101));
#12874=CARTESIAN_POINT('Ctrl Pts',(-204.535482847057,-97.615167925323,11.3884295143086));
#12875=CARTESIAN_POINT('Ctrl Pts',(-205.485485371038,-97.6113566239648,
11.3354600747072));
#12876=CARTESIAN_POINT('Ctrl Pts',(-206.216148018684,-97.2091172546447,
11.2824906351058));
#12877=CARTESIAN_POINT('Ctrl Pts',(-206.946810666331,-96.8068778853247,
11.2295211955043));
#12878=CARTESIAN_POINT('Ctrl Pts',(-207.458133437644,-96.0062104480429,
11.1765517559029));
#12879=CARTESIAN_POINT('Ctrl Pts',(-207.515728831729,-95.1741364216021,
11.1235823163015));
#12880=CARTESIAN_POINT('Ctrl Pts',(-207.573324225813,-94.3420623951613,
11.0706128767));
#12881=CARTESIAN_POINT('Ctrl Pts',(-207.177192242668,-93.4785817795614,
11.0176434370986));
#12882=CARTESIAN_POINT('Ctrl Pts',(-206.508917569625,-92.9795092635214,
10.9646739974971));
#12883=CARTESIAN_POINT('Ctrl Pts',(-205.840642896582,-92.4804367474813,
10.9117045578957));
#12884=CARTESIAN_POINT('Ctrl Pts',(-204.900225533641,-92.3457723310011,
10.8587351182943));
#12885=CARTESIAN_POINT('Ctrl Pts',(-204.118747544549,-92.6372454300371,
10.8057656786928));
#12886=CARTESIAN_POINT('Ctrl Pts',(-203.337269555457,-92.9287185290731,
10.7527962390914));
#12887=CARTESIAN_POINT('Ctrl Pts',(-202.714730940213,-93.6463291436252,
10.69982679949));
#12888=CARTESIAN_POINT('Ctrl Pts',(-202.536499921054,-94.4611285782756,
10.6468573598885));
#12889=CARTESIAN_POINT('Ctrl Pts',(-202.498058257166,-94.6368681669895,
10.6354326740897));
#12890=CARTESIAN_POINT('Ctrl Pts',(-202.480285690666,-94.8171289594943,
10.6240079882908));
#12891=CARTESIAN_POINT('Ctrl Pts',(-202.481958443618,-94.9977164072965,
10.612583302492));
#12892=CARTESIAN_POINT('Origin',(-205.,-95.,9.));
#12893=CARTESIAN_POINT('',(-202.486537790415,-95.0001194277165,9.61258330249196));
#12894=CARTESIAN_POINT('',(-202.482602555105,-95.0023130495141,9.88741669750803));
#12895=CARTESIAN_POINT('',(-202.4825,-95.,9.));
#12896=CARTESIAN_POINT('Ctrl Pts',(-202.482602555105,-95.0023130495141,
9.88741669750803));
#12897=CARTESIAN_POINT('Ctrl Pts',(-202.488423652239,-94.3663734982534,
9.92762245587553));
#12898=CARTESIAN_POINT('Ctrl Pts',(-202.733269661135,-93.7264433715794,
9.96782821424302));
#12899=CARTESIAN_POINT('Ctrl Pts',(-203.168433552404,-93.2666277755833,
10.0080339726105));
#12900=CARTESIAN_POINT('Ctrl Pts',(-203.741744152458,-92.66083956442,10.061003412212));
#12901=CARTESIAN_POINT('Ctrl Pts',(-204.645389178865,-92.3676758393408,
10.1139728518134));
#12902=CARTESIAN_POINT('Ctrl Pts',(-205.465142801446,-92.5215212136069,
10.1669422914148));
#12903=CARTESIAN_POINT('Ctrl Pts',(-206.284896424028,-92.675366587873,10.2199117310163));
#12904=CARTESIAN_POINT('Ctrl Pts',(-207.020758642784,-93.2762210614844,
10.2728811706177));
#12905=CARTESIAN_POINT('Ctrl Pts',(-207.335414328927,-94.0486563015507,
10.3258506102191));
#12906=CARTESIAN_POINT('Ctrl Pts',(-207.65007001507,-94.821091541617,10.3788200498206));
#12907=CARTESIAN_POINT('Ctrl Pts',(-207.543519168601,-95.7651075481382,
10.431789489422));
#12908=CARTESIAN_POINT('Ctrl Pts',(-207.064604102091,-96.4479726592609,
10.4847589290234));
#12909=CARTESIAN_POINT('Ctrl Pts',(-206.585689035581,-97.1308377703837,
10.5377283686249));
#12910=CARTESIAN_POINT('Ctrl Pts',(-205.734409749032,-97.5525519861079,
10.5906978082263));
#12911=CARTESIAN_POINT('Ctrl Pts',(-204.900987910111,-97.5198038666518,
10.6436672478277));
#12912=CARTESIAN_POINT('Ctrl Pts',(-204.06756607119,-97.4870557471958,10.6966366874292));
#12913=CARTESIAN_POINT('Ctrl Pts',(-203.252001679897,-96.9998452925596,
10.7496061270306));
#12914=CARTESIAN_POINT('Ctrl Pts',(-202.828144895504,-96.2815070524231,
10.8025755666321));
#12915=CARTESIAN_POINT('Ctrl Pts',(-202.601847813085,-95.8979863588357,
10.8308559435907));
#12916=CARTESIAN_POINT('Ctrl Pts',(-202.487206620518,-95.4485829044729,
10.8591363205494));
#12917=CARTESIAN_POINT('Ctrl Pts',(-202.486464107889,-94.9995333136293,
10.887416697508));
#12918=CARTESIAN_POINT('Ctrl Pts',(-202.481958443618,-94.9977164072965,
10.612583302492));
#12919=CARTESIAN_POINT('Ctrl Pts',(-202.488041246315,-95.6544050192081,
10.5710385486894));
#12920=CARTESIAN_POINT('Ctrl Pts',(-202.751257709045,-96.3154131318815,
10.5294937948868));
#12921=CARTESIAN_POINT('Ctrl Pts',(-203.212761635906,-96.7790430230964,
10.4879490410842));
#12922=CARTESIAN_POINT('Ctrl Pts',(-203.801177792993,-97.3701697785185,
10.4349796014828));
#12923=CARTESIAN_POINT('Ctrl Pts',(-204.711933530243,-97.6404350346142,
10.3820101618814));
#12924=CARTESIAN_POINT('Ctrl Pts',(-205.527543507365,-97.4659507083387,
10.3290407222799));
#12925=CARTESIAN_POINT('Ctrl Pts',(-206.343153484488,-97.2914663820631,
10.2760712826785));
#12926=CARTESIAN_POINT('Ctrl Pts',(-207.063617701482,-96.6722324734162,
10.223101843077));
#12927=CARTESIAN_POINT('Ctrl Pts',(-207.358679387517,-95.8921023455972,
10.1701324034756));
#12928=CARTESIAN_POINT('Ctrl Pts',(-207.653741073553,-95.1119722177781,
10.1171629638742));
#12929=CARTESIAN_POINT('Ctrl Pts',(-207.52340022863,-94.1709458707869,10.0641935242727));
#12930=CARTESIAN_POINT('Ctrl Pts',(-207.027404367665,-93.5003845232557,
10.0112240846713));
#12931=CARTESIAN_POINT('Ctrl Pts',(-206.5314085067,-92.8298231757246,9.95825464506987));
#12932=CARTESIAN_POINT('Ctrl Pts',(-205.669757629693,-92.4297268276535,
9.90528520546843));
#12933=CARTESIAN_POINT('Ctrl Pts',(-204.837427683417,-92.4834974091013,
9.852315765867));
#12934=CARTESIAN_POINT('Ctrl Pts',(-204.005097737141,-92.537267990549,9.79934632626556));
#12935=CARTESIAN_POINT('Ctrl Pts',(-203.202088721596,-93.0449055015156,
9.74637688666412));
#12936=CARTESIAN_POINT('Ctrl Pts',(-202.796495481975,-93.7737117438536,
9.69340744706269));
#12937=CARTESIAN_POINT('Ctrl Pts',(-202.590202149551,-94.1443980712782,
9.66646606553911));
#12938=CARTESIAN_POINT('Ctrl Pts',(-202.486718512095,-94.5722997665523,
9.63952468401554));
#12939=CARTESIAN_POINT('Ctrl Pts',(-202.486537790415,-95.0001194277165,
9.61258330249196));
#12940=CARTESIAN_POINT('Origin',(-205.,-95.,9.));
#12941=CARTESIAN_POINT('',(-202.48151911239,-95.0022302404453,8.61258330249196));
#12942=CARTESIAN_POINT('',(-202.478554974092,-94.9992065476435,8.88741669750803));
#12943=CARTESIAN_POINT('',(-202.4825,-95.,9.));
#12944=CARTESIAN_POINT('Ctrl Pts',(-202.478554974092,-94.9992065476435,
8.88741669750803));
#12945=CARTESIAN_POINT('Ctrl Pts',(-202.478376117211,-94.9558431822019,
8.89016971199881));
#12946=CARTESIAN_POINT('Ctrl Pts',(-202.47939772805,-94.9124884193367,8.89292272648959));
#12947=CARTESIAN_POINT('Ctrl Pts',(-202.481646252911,-94.8691973820566,
8.89567574098037));
#12948=CARTESIAN_POINT('Ctrl Pts',(-202.524909048014,-94.0362551682876,
8.94864518058181));
#12949=CARTESIAN_POINT('Ctrl Pts',(-203.022372640194,-93.2269040220556,
9.00161462018325));
#12950=CARTESIAN_POINT('Ctrl Pts',(-203.74600249882,-92.8121459858182,9.05458405978468));
#12951=CARTESIAN_POINT('Ctrl Pts',(-204.469632357446,-92.3973879495807,
9.10755349938612));
#12952=CARTESIAN_POINT('Ctrl Pts',(-205.419428482518,-92.3772230233378,
9.16052293898755));
#12953=CARTESIAN_POINT('Ctrl Pts',(-206.16000963814,-92.7608946965896,9.21349237858899));
#12954=CARTESIAN_POINT('Ctrl Pts',(-206.900590793762,-93.1445663698413,
9.26646181819042));
#12955=CARTESIAN_POINT('Ctrl Pts',(-207.431956979935,-93.9320746425879,
9.31943125779186));
#12956=CARTESIAN_POINT('Ctrl Pts',(-207.510532906401,-94.7624301235107,
9.3724006973933));
#12957=CARTESIAN_POINT('Ctrl Pts',(-207.589108832868,-95.5927856044335,
9.42537013699473));
#12958=CARTESIAN_POINT('Ctrl Pts',(-207.214894499628,-96.4659882935325,
9.47833957659616));
#12959=CARTESIAN_POINT('Ctrl Pts',(-206.559427665781,-96.9817669579278,
9.5313090161976));
#12960=CARTESIAN_POINT('Ctrl Pts',(-205.903960831934,-97.497545622323,9.58427845579904));
#12961=CARTESIAN_POINT('Ctrl Pts',(-204.96724149748,-97.6559002620145,9.63724789540048));
#12962=CARTESIAN_POINT('Ctrl Pts',(-204.178656570574,-97.3842419951162,
9.69021733500191));
#12963=CARTESIAN_POINT('Ctrl Pts',(-203.390071643667,-97.1125837282179,
9.74318677460335));
#12964=CARTESIAN_POINT('Ctrl Pts',(-202.749621124308,-96.4109125547298,
9.79615621420478));
#12965=CARTESIAN_POINT('Ctrl Pts',(-202.550883951478,-95.600870619362,9.84912565380621));
#12966=CARTESIAN_POINT('Ctrl Pts',(-202.502995622993,-95.4056803902987,
9.86188933504015));
#12967=CARTESIAN_POINT('Ctrl Pts',(-202.480754595229,-95.2041978054776,
9.87465301627409));
#12968=CARTESIAN_POINT('Ctrl Pts',(-202.482602555105,-95.0023130495141,
9.88741669750803));
#12969=CARTESIAN_POINT('Ctrl Pts',(-202.486537790415,-95.0001194277165,
9.61258330249196));
#12970=CARTESIAN_POINT('Ctrl Pts',(-202.486363195271,-95.4134358338514,
9.5865552444141));
#12971=CARTESIAN_POINT('Ctrl Pts',(-202.582606216335,-95.826675673577,9.56052718633624));
#12972=CARTESIAN_POINT('Ctrl Pts',(-202.775711594544,-96.1881734458707,
9.53449912825838));
#12973=CARTESIAN_POINT('Ctrl Pts',(-203.168698410431,-96.9238539318402,
9.48152968865694));
#12974=CARTESIAN_POINT('Ctrl Pts',(-203.962849505901,-97.4452399300696,
9.4285602490555));
#12975=CARTESIAN_POINT('Ctrl Pts',(-204.794130456823,-97.5133310126825,
9.37559080945407));
#12976=CARTESIAN_POINT('Ctrl Pts',(-205.625411407745,-97.5814220952953,
9.32262136985264));
#12977=CARTESIAN_POINT('Ctrl Pts',(-206.493822214119,-97.1962182622914,
9.26965193025121));
#12978=CARTESIAN_POINT('Ctrl Pts',(-207.001288215326,-96.5342947980481,
9.21668249064977));
#12979=CARTESIAN_POINT('Ctrl Pts',(-207.508754216533,-95.8723713338047,
9.16371305104833));
#12980=CARTESIAN_POINT('Ctrl Pts',(-207.655275412574,-94.9337282383218,
9.11074361144689));
#12981=CARTESIAN_POINT('Ctrl Pts',(-207.373687306002,-94.1486342610589,
9.05777417184546));
#12982=CARTESIAN_POINT('Ctrl Pts',(-207.092099199431,-93.363540283796,9.00480473224402));
#12983=CARTESIAN_POINT('Ctrl Pts',(-206.382401790246,-92.7319954247531,
8.95183529264259));
#12984=CARTESIAN_POINT('Ctrl Pts',(-205.569916404748,-92.5434963179922,
8.89886585304116));
#12985=CARTESIAN_POINT('Ctrl Pts',(-204.75743101925,-92.3549972112313,8.84589641343972));
#12986=CARTESIAN_POINT('Ctrl Pts',(-203.842157657439,-92.6095438567524,
8.79292697383828));
#12987=CARTESIAN_POINT('Ctrl Pts',(-203.243652513459,-93.1904534947564,
8.73995753423685));
#12988=CARTESIAN_POINT('Ctrl Pts',(-202.763915936522,-93.6560862533854,
8.69749945698855));
#12989=CARTESIAN_POINT('Ctrl Pts',(-202.487701419864,-94.3314056689759,
8.65504137974025));
#12990=CARTESIAN_POINT('Ctrl Pts',(-202.48151911239,-95.0022302404453,8.61258330249196));
#12991=CARTESIAN_POINT('Origin',(-205.,-95.,9.));
#12992=CARTESIAN_POINT('',(-202.479176535286,-94.9986328420086,7.61258330249196));
#12993=CARTESIAN_POINT('',(-202.484976587536,-94.9981409198179,7.88741669750803));
#12994=CARTESIAN_POINT('',(-202.4825,-95.,9.));
#12995=CARTESIAN_POINT('Ctrl Pts',(-202.484976587536,-94.9981409198179,
7.88741669750803));
#12996=CARTESIAN_POINT('Ctrl Pts',(-202.482996634039,-94.7084750992777,
7.90568640772353));
#12997=CARTESIAN_POINT('Ctrl Pts',(-202.529190054397,-94.4194213389179,
7.92395611793903));
#12998=CARTESIAN_POINT('Ctrl Pts',(-202.626312717846,-94.1486342696126,
7.94222582815454));
#12999=CARTESIAN_POINT('Ctrl Pts',(-202.907900821589,-93.3635403002374,
7.99519526775597));
#13000=CARTESIAN_POINT('Ctrl Pts',(-203.617598223643,-92.7319954475396,
8.04816470735741));
#13001=CARTESIAN_POINT('Ctrl Pts',(-204.430083600978,-92.5434963426725,
8.10113414695884));
#13002=CARTESIAN_POINT('Ctrl Pts',(-205.242568978313,-92.3549972378055,
8.15410358656028));
#13003=CARTESIAN_POINT('Ctrl Pts',(-206.157842330928,-92.6095438807692,
8.20707302616171));
#13004=CARTESIAN_POINT('Ctrl Pts',(-206.756347468895,-93.1904535129367,
8.26004246576315));
#13005=CARTESIAN_POINT('Ctrl Pts',(-207.354852606863,-93.7713631451043,
8.31301190536458));
#13006=CARTESIAN_POINT('Ctrl Pts',(-207.636589530182,-94.6786357664758,
8.36598134496602));
#13007=CARTESIAN_POINT('Ctrl Pts',(-207.472411607662,-95.4963826776137,
8.41895078456746));
#13008=CARTESIAN_POINT('Ctrl Pts',(-207.308233685142,-96.3141295887515,
8.47192022416889));
#13009=CARTESIAN_POINT('Ctrl Pts',(-206.698140916782,-97.0423507896557,
8.52488966377032));
#13010=CARTESIAN_POINT('Ctrl Pts',(-205.921796418158,-97.3472337514208,
8.57785910337176));
#13011=CARTESIAN_POINT('Ctrl Pts',(-205.145451919534,-97.6521167131859,
8.6308285429732));
#13012=CARTESIAN_POINT('Ctrl Pts',(-204.202855690646,-97.5336614358119,
8.68379798257464));
#13013=CARTESIAN_POINT('Ctrl Pts',(-203.526088575214,-97.0461671564718,
8.73676742217607));
#13014=CARTESIAN_POINT('Ctrl Pts',(-202.884495509002,-96.5840097284425,
8.78698384728673));
#13015=CARTESIAN_POINT('Ctrl Pts',(-202.481817417207,-95.7901770276534,
8.83720027239738));
#13016=CARTESIAN_POINT('Ctrl Pts',(-202.478554974092,-94.9992065476435,
8.88741669750803));
#13017=CARTESIAN_POINT('Ctrl Pts',(-202.48151911239,-95.0022302404453,8.61258330249196));
#13018=CARTESIAN_POINT('Ctrl Pts',(-202.479988556174,-95.1683065350657,
8.60207194013882));
#13019=CARTESIAN_POINT('Ctrl Pts',(-202.495008569329,-95.334107335775,8.59156057778568));
#13020=CARTESIAN_POINT('Ctrl Pts',(-202.527588367498,-95.4963826826008,
8.58104921543254));
#13021=CARTESIAN_POINT('Ctrl Pts',(-202.691766291667,-96.3141296019545,
8.5280797758311));
#13022=CARTESIAN_POINT('Ctrl Pts',(-203.301859066157,-97.0423508101752,
8.47511033622967));
#13023=CARTESIAN_POINT('Ctrl Pts',(-204.078203572581,-97.3472337750034,
8.42214089662823));
#13024=CARTESIAN_POINT('Ctrl Pts',(-204.854548079005,-97.6521167398316,
8.36917145702679));
#13025=CARTESIAN_POINT('Ctrl Pts',(-205.797144317363,-97.5336614612674,
8.31620201742536));
#13026=CARTESIAN_POINT('Ctrl Pts',(-206.473911439594,-97.0461671770295,
8.26323257782393));
#13027=CARTESIAN_POINT('Ctrl Pts',(-207.150678561825,-96.5586728927915,
8.21026313822249));
#13028=CARTESIAN_POINT('Ctrl Pts',(-207.561616567928,-95.70213960288,8.15729369862105));
#13029=CARTESIAN_POINT('Ctrl Pts',(-207.518353772391,-94.8691973807424,
8.10432425901962));
#13030=CARTESIAN_POINT('Ctrl Pts',(-207.475090976853,-94.0362551586049,
8.05135481941818));
#13031=CARTESIAN_POINT('Ctrl Pts',(-206.977627379675,-93.2269040042414,
7.99838537981675));
#13032=CARTESIAN_POINT('Ctrl Pts',(-206.253997513779,-92.8121459638369,
7.94541594021531));
#13033=CARTESIAN_POINT('Ctrl Pts',(-205.530367647883,-92.3973879234324,
7.89244650061388));
#13034=CARTESIAN_POINT('Ctrl Pts',(-204.580571513268,-92.3772229969869,
7.83947706101244));
#13035=CARTESIAN_POINT('Ctrl Pts',(-203.839990350206,-92.7608946740935,
7.78650762141101));
#13036=CARTESIAN_POINT('Ctrl Pts',(-203.099409187143,-93.1445663512,7.73353818180957));
#13037=CARTESIAN_POINT('Ctrl Pts',(-202.568042995632,-93.9320746318586,
7.68056874220814));
#13038=CARTESIAN_POINT('Ctrl Pts',(-202.489467068376,-94.7624301211239,
7.6275993026067));
#13039=CARTESIAN_POINT('Ctrl Pts',(-202.482042056636,-94.8408943463822,
7.62259396923512));
#13040=CARTESIAN_POINT('Ctrl Pts',(-202.478660124946,-94.9197411653224,
7.61758863586354));
#13041=CARTESIAN_POINT('Ctrl Pts',(-202.479176535286,-94.9986328420086,
7.61258330249196));
#13042=CARTESIAN_POINT('Origin',(-205.,-95.,9.));
#13043=CARTESIAN_POINT('',(-202.485695966289,-94.9985525878773,6.61258330249196));
#13044=CARTESIAN_POINT('',(-202.48529106324,-95.001705225411,6.88741669750803));
#13045=CARTESIAN_POINT('',(-202.4825,-95.,9.));
#13046=CARTESIAN_POINT('Ctrl Pts',(-202.48529106324,-95.001705225411,6.88741669750803));
#13047=CARTESIAN_POINT('Ctrl Pts',(-202.488622939146,-94.465854223785,6.92120310344825));
#13048=CARTESIAN_POINT('Ctrl Pts',(-202.656226110927,-93.9281001765914,
6.95498950938847));
#13049=CARTESIAN_POINT('Ctrl Pts',(-202.972595652704,-93.5003845383223,
6.9887759153287));
#13050=CARTESIAN_POINT('Ctrl Pts',(-203.468591508686,-92.8298231975282,
7.04174535493013));
#13051=CARTESIAN_POINT('Ctrl Pts',(-204.330242377036,-92.429726853477,7.09471479453157));
#13052=CARTESIAN_POINT('Ctrl Pts',(-205.162572314949,-92.4834974343845,
7.14768423413301));
#13053=CARTESIAN_POINT('Ctrl Pts',(-205.994902252863,-92.537268015292,7.20065367373444));
#13054=CARTESIAN_POINT('Ctrl Pts',(-206.797911260341,-93.0449055211583,
7.25362311333587));
#13055=CARTESIAN_POINT('Ctrl Pts',(-207.203504495887,-93.773711756174,7.30659255293731));
#13056=CARTESIAN_POINT('Ctrl Pts',(-207.609097731433,-94.5025179911897,
7.35956199253874));
#13057=CARTESIAN_POINT('Ctrl Pts',(-207.617275195047,-95.452492955355,7.41253143214018));
#13058=CARTESIAN_POINT('Ctrl Pts',(-207.224288383109,-96.1881734339332,
7.46550087174162));
#13059=CARTESIAN_POINT('Ctrl Pts',(-206.83130157117,-96.9238539125113,7.51847031134306));
#13060=CARTESIAN_POINT('Ctrl Pts',(-206.037150483679,-97.4452399055024,
7.57143975094449));
#13061=CARTESIAN_POINT('Ctrl Pts',(-205.205869541108,-97.5133309874311,
7.62440919054592));
#13062=CARTESIAN_POINT('Ctrl Pts',(-204.374588598538,-97.5814220693598,
7.67737863014736));
#13063=CARTESIAN_POINT('Ctrl Pts',(-203.50617780089,-97.1962182402261,7.7303480697488));
#13064=CARTESIAN_POINT('Ctrl Pts',(-202.998711804781,-96.5342947826331,
7.78331750935023));
#13065=CARTESIAN_POINT('Ctrl Pts',(-202.666276104686,-96.1006756047542,
7.81801723873617));
#13066=CARTESIAN_POINT('Ctrl Pts',(-202.488737120666,-95.5483043031743,
7.8527169681221));
#13067=CARTESIAN_POINT('Ctrl Pts',(-202.484976587536,-94.9981409198179,
7.88741669750803));
#13068=CARTESIAN_POINT('Ctrl Pts',(-202.479176535286,-94.9986328420086,
7.61258330249196));
#13069=CARTESIAN_POINT('Ctrl Pts',(-202.484125088871,-95.7546202019532,
7.5646191962621));
#13070=CARTESIAN_POINT('Ctrl Pts',(-202.847043646147,-96.514726679039,7.51665509003225));
#13071=CARTESIAN_POINT('Ctrl Pts',(-203.440572318551,-96.9817669778385,
7.46869098380239));
#13072=CARTESIAN_POINT('Ctrl Pts',(-204.096039158984,-97.4975456474158,
7.41572154420096));
#13073=CARTESIAN_POINT('Ctrl Pts',(-205.032758502849,-97.6559002886982,
7.36275210459952));
#13074=CARTESIAN_POINT('Ctrl Pts',(-205.821343437678,-97.3842420190706,
7.30978266499809));
#13075=CARTESIAN_POINT('Ctrl Pts',(-206.609928372508,-97.1125837494429,
7.25681322539665));
#13076=CARTESIAN_POINT('Ctrl Pts',(-207.250378898302,-96.4109125689051,
7.20384378579521));
#13077=CARTESIAN_POINT('Ctrl Pts',(-207.449116073128,-95.6008706253988,
7.15087434619378));
#13078=CARTESIAN_POINT('Ctrl Pts',(-207.647853247953,-94.7908286818925,
7.09790490659234));
#13079=CARTESIAN_POINT('Ctrl Pts',(-207.404877071811,-93.8724159754179,
7.04493546699091));
#13080=CARTESIAN_POINT('Ctrl Pts',(-206.831566465997,-93.2666277581682,
6.99196602738948));
#13081=CARTESIAN_POINT('Ctrl Pts',(-206.258255860184,-92.6608395409186,
6.93899658778804));
#13082=CARTESIAN_POINT('Ctrl Pts',(-205.354610824698,-92.367675812894,6.8860271481866));
#13083=CARTESIAN_POINT('Ctrl Pts',(-204.53485719388,-92.5215211887057,6.83305770858517));
#13084=CARTESIAN_POINT('Ctrl Pts',(-203.715103563063,-92.6753665645175,
6.78008826898373));
#13085=CARTESIAN_POINT('Ctrl Pts',(-202.979241336913,-93.2762210441657,
6.72711882938229));
#13086=CARTESIAN_POINT('Ctrl Pts',(-202.664585647609,-94.0486562919927,
6.67414938978086));
#13087=CARTESIAN_POINT('Ctrl Pts',(-202.542678123954,-94.3479220337145,
6.65362736068456));
#13088=CARTESIAN_POINT('Ctrl Pts',(-202.48399503341,-94.6729425913092,6.63310533158826));
#13089=CARTESIAN_POINT('Ctrl Pts',(-202.485695966289,-94.9985525878773,
6.61258330249196));
#13090=CARTESIAN_POINT('Origin',(-205.,-95.,9.));
#13091=CARTESIAN_POINT('',(-202.484465718496,-95.0020481324837,5.61258330249196));
#13092=CARTESIAN_POINT('',(-202.478772638074,-95.0010375285769,5.88741669750803));
#13093=CARTESIAN_POINT('',(-202.4825,-95.,9.));
#13094=CARTESIAN_POINT('Ctrl Pts',(-202.478772638074,-95.0010375285769,
5.88741669750803));
#13095=CARTESIAN_POINT('Ctrl Pts',(-202.482817019795,-94.2242747158738,
5.93671979917297));
#13096=CARTESIAN_POINT('Ctrl Pts',(-202.869063144179,-93.4440379428825,
5.98602290083791));
#13097=CARTESIAN_POINT('Ctrl Pts',(-203.491082445535,-92.9795092838211,
6.03532600250286));
#13098=CARTESIAN_POINT('Ctrl Pts',(-204.159357111864,-92.4804367727953,
6.08829544210429));
#13099=CARTESIAN_POINT('Ctrl Pts',(-205.099774465356,-92.345772357668,6.14126488170573));
#13100=CARTESIAN_POINT('Ctrl Pts',(-205.881252446597,-92.6372454537756,
6.19423432130716));
#13101=CARTESIAN_POINT('Ctrl Pts',(-206.662730427838,-92.9287185498831,
6.2472037609086));
#13102=CARTESIAN_POINT('Ctrl Pts',(-207.285269036827,-93.6463291572254,
6.30017320051003));
#13103=CARTESIAN_POINT('Ctrl Pts',(-207.463500054196,-94.4611285836895,
6.35314264011147));
#13104=CARTESIAN_POINT('Ctrl Pts',(-207.641731071564,-95.2759280101535,
6.4061120797129));
#13105=CARTESIAN_POINT('Ctrl Pts',(-207.375654497314,-96.1879162557393,
6.45908151931434));
#13106=CARTESIAN_POINT('Ctrl Pts',(-206.787238346138,-96.7790430052224,
6.51205095891577));
#13107=CARTESIAN_POINT('Ctrl Pts',(-206.198822194963,-97.3701697547055,
6.56502039851721));
#13108=CARTESIAN_POINT('Ctrl Pts',(-205.288066466863,-97.6404350080859,
6.61798983811865));
#13109=CARTESIAN_POINT('Ctrl Pts',(-204.472456497935,-97.4659506835634,
6.67095927772009));
#13110=CARTESIAN_POINT('Ctrl Pts',(-203.656846529007,-97.2914663590408,
6.72392871732152));
#13111=CARTESIAN_POINT('Ctrl Pts',(-202.936382319251,-96.6722324566154,
6.77689815692296));
#13112=CARTESIAN_POINT('Ctrl Pts',(-202.64132063618,-95.8921023366343,6.82986759652439));
#13113=CARTESIAN_POINT('Ctrl Pts',(-202.534463205913,-95.6095759881524,
6.84905063018561));
#13114=CARTESIAN_POINT('Ctrl Pts',(-202.483399311635,-95.305947346333,6.86823366384682));
#13115=CARTESIAN_POINT('Ctrl Pts',(-202.48529106324,-95.001705225411,6.88741669750803));
#13116=CARTESIAN_POINT('Ctrl Pts',(-202.485695966289,-94.9985525878773,
6.61258330249196));
#13117=CARTESIAN_POINT('Ctrl Pts',(-202.488385313776,-95.5133750342175,
6.58013589198682));
#13118=CARTESIAN_POINT('Ctrl Pts',(-202.642027587202,-96.0296710083661,
6.54768848148169));
#13119=CARTESIAN_POINT('Ctrl Pts',(-202.935395877166,-96.4479726738087,
6.51524107097655));
#13120=CARTESIAN_POINT('Ctrl Pts',(-203.414310948487,-97.1308377917921,
6.46227163137512));
#13121=CARTESIAN_POINT('Ctrl Pts',(-204.26559024359,-97.5525520117532,6.40930219177368));
#13122=CARTESIAN_POINT('Ctrl Pts',(-205.099012090884,-97.5198038919682,
6.35633275217224));
#13123=CARTESIAN_POINT('Ctrl Pts',(-205.932433938178,-97.4870557721831,
6.30336331257081));
#13124=CARTESIAN_POINT('Ctrl Pts',(-206.747998337665,-96.9998453126519,
6.25039387296938));
#13125=CARTESIAN_POINT('Ctrl Pts',(-207.171855126317,-96.2815070652983,
6.19742443336794));
#13126=CARTESIAN_POINT('Ctrl Pts',(-207.595711914969,-95.5631688179448,
6.14445499376651));
#13127=CARTESIAN_POINT('Ctrl Pts',(-207.627861092786,-94.6137027827689,
6.09148555416507));
#13128=CARTESIAN_POINT('Ctrl Pts',(-207.253565656318,-93.8683388843025,
6.03851611456364));
#13129=CARTESIAN_POINT('Ctrl Pts',(-206.879270219851,-93.1229749858362,
5.9855466749622));
#13130=CARTESIAN_POINT('Ctrl Pts',(-206.0985301691,-92.5817132240792,5.93257723536076));
#13131=CARTESIAN_POINT('Ctrl Pts',(-205.269232380244,-92.4926649658358,
5.87960779575933));
#13132=CARTESIAN_POINT('Ctrl Pts',(-204.439934591389,-92.4036167075924,
5.82663835615789));
#13133=CARTESIAN_POINT('Ctrl Pts',(-203.562079064428,-92.7667819528624,
5.77366891655646));
#13134=CARTESIAN_POINT('Ctrl Pts',(-203.038069867117,-93.4156877827256,
5.72069947695502));
#13135=CARTESIAN_POINT('Ctrl Pts',(-202.681550647588,-93.8571827053293,
5.684660752134));
#13136=CARTESIAN_POINT('Ctrl Pts',(-202.488827231246,-94.430947216833,5.64862202731298));
#13137=CARTESIAN_POINT('Ctrl Pts',(-202.484465718496,-95.0020481324837,
5.61258330249196));
#13138=CARTESIAN_POINT('Origin',(-205.,-95.,9.));
#13139=CARTESIAN_POINT('',(-202.478335348143,-95.0004148939562,4.61258330249195));
#13140=CARTESIAN_POINT('',(-202.482163763775,-94.997700765499,4.88741669750803));
#13141=CARTESIAN_POINT('',(-202.4825,-95.,9.));
#13142=CARTESIAN_POINT('Ctrl Pts',(-202.482163763775,-94.997700765499,4.88741669750803));
#13143=CARTESIAN_POINT('Ctrl Pts',(-202.480430648174,-94.8103456723384,
4.89926705529626));
#13144=CARTESIAN_POINT('Ctrl Pts',(-202.499567671021,-94.6233413479286,
4.91111741308448));
#13145=CARTESIAN_POINT('Ctrl Pts',(-202.540902956965,-94.4413796877348,
4.92296777087271));
#13146=CARTESIAN_POINT('Ctrl Pts',(-202.725665895886,-93.6280365514634,
4.97593721047414));
#13147=CARTESIAN_POINT('Ctrl Pts',(-203.353942315917,-92.9154440708087,
5.02890665007558));
#13148=CARTESIAN_POINT('Ctrl Pts',(-204.137733817173,-92.6302506566537,
5.08187608967701));
#13149=CARTESIAN_POINT('Ctrl Pts',(-204.921525318429,-92.3450572424987,
5.13484552927845));
#13150=CARTESIAN_POINT('Ctrl Pts',(-205.86083190091,-92.4872628948432,5.18781496887989));
#13151=CARTESIAN_POINT('Ctrl Pts',(-206.525080676425,-92.9916813373541,
5.24078440848132));
#13152=CARTESIAN_POINT('Ctrl Pts',(-207.189329451941,-93.496099779865,5.29375384808276));
#13153=CARTESIAN_POINT('Ctrl Pts',(-207.578520420489,-94.3627310125423,
5.34672328768419));
#13154=CARTESIAN_POINT('Ctrl Pts',(-207.514250617043,-95.1943161214058,
5.39969272728563));
#13155=CARTESIAN_POINT('Ctrl Pts',(-207.449980813596,-96.0259012302693,
5.45266216688706));
#13156=CARTESIAN_POINT('Ctrl Pts',(-206.932250238154,-96.8224402153189,
5.5056316064885));
#13157=CARTESIAN_POINT('Ctrl Pts',(-206.198383693215,-97.2188040571838,
5.55860104608993));
#13158=CARTESIAN_POINT('Ctrl Pts',(-205.464517148276,-97.6151678990486,
5.61157048569137));
#13159=CARTESIAN_POINT('Ctrl Pts',(-204.51451463384,-97.6113565977286,5.66453992529281));
#13160=CARTESIAN_POINT('Ctrl Pts',(-203.783851993534,-97.2091172324499,
5.71750936489424));
#13161=CARTESIAN_POINT('Ctrl Pts',(-203.053189353228,-96.8068778671711,
5.77047880449568));
#13162=CARTESIAN_POINT('Ctrl Pts',(-202.541866587052,-96.0062104379335,
5.82344824409711));
#13163=CARTESIAN_POINT('Ctrl Pts',(-202.484271193547,-95.1741364198525,
5.87641768369855));
#13164=CARTESIAN_POINT('Ctrl Pts',(-202.48028466513,-95.1165435028532,5.88008402163504));
#13165=CARTESIAN_POINT('Ctrl Pts',(-202.478471884782,-95.0588001210244,
5.88375035957154));
#13166=CARTESIAN_POINT('Ctrl Pts',(-202.478772638074,-95.0010375285769,
5.88741669750803));
#13167=CARTESIAN_POINT('Ctrl Pts',(-202.484465718496,-95.0020481324837,
5.61258330249196));
#13168=CARTESIAN_POINT('Ctrl Pts',(-202.482416713467,-95.2703469350006,
5.59565258771154));
#13169=CARTESIAN_POINT('Ctrl Pts',(-202.521940082511,-95.5380578691583,
5.57872187293113));
#13170=CARTESIAN_POINT('Ctrl Pts',(-202.605582971729,-95.7911903328824,
5.56179115815071));
#13171=CARTESIAN_POINT('Ctrl Pts',(-202.867268141315,-96.5831406387199,
5.50882171854928));
#13172=CARTESIAN_POINT('Ctrl Pts',(-203.560801348149,-97.2323948359386,
5.45585227894784));
#13173=CARTESIAN_POINT('Ctrl Pts',(-204.368270845956,-97.4413384288235,
5.40288283934641));
#13174=CARTESIAN_POINT('Ctrl Pts',(-205.175740343764,-97.6502820217083,
5.34991339974497));
#13175=CARTESIAN_POINT('Ctrl Pts',(-206.097146132545,-97.4189150102591,
5.29694396014354));
#13176=CARTESIAN_POINT('Ctrl Pts',(-206.710120947904,-96.8532947395539,
5.2439745205421));
#13177=CARTESIAN_POINT('Ctrl Pts',(-207.323095763263,-96.2876744688487,
5.19100508094066));
#13178=CARTESIAN_POINT('Ctrl Pts',(-207.6276396052,-95.3878009388875,5.13803564133923));
#13179=CARTESIAN_POINT('Ctrl Pts',(-207.484151278482,-94.5661711469537,
5.08506620173779));
#13180=CARTESIAN_POINT('Ctrl Pts',(-207.340662951764,-93.74454135502,5.03209676213636));
#13181=CARTESIAN_POINT('Ctrl Pts',(-206.749142456392,-93.0011553011137,
4.97912732253492));
#13182=CARTESIAN_POINT('Ctrl Pts',(-205.980739481793,-92.6767769980105,
4.92615788293349));
#13183=CARTESIAN_POINT('Ctrl Pts',(-205.212336507194,-92.3523986949072,
4.87318844333205));
#13184=CARTESIAN_POINT('Ctrl Pts',(-204.267051053368,-92.447028142607,4.82021900373062));
#13185=CARTESIAN_POINT('Ctrl Pts',(-203.578196689718,-92.917287731109,4.76724956412918));
#13186=CARTESIAN_POINT('Ctrl Pts',(-202.907731291558,-93.3749937410897,
4.71569414358344));
#13187=CARTESIAN_POINT('Ctrl Pts',(-202.480188867636,-94.1885426831987,
4.6641387230377));
#13188=CARTESIAN_POINT('Ctrl Pts',(-202.478335348143,-95.0004148939562,
4.61258330249195));
#13189=CARTESIAN_POINT('Origin',(-205.,-95.,9.));
#13190=CARTESIAN_POINT('',(-202.483233733754,-94.9977147790846,3.61258330249195));
#13191=CARTESIAN_POINT('',(-202.486523858474,-95.0002304794208,3.88741669750803));
#13192=CARTESIAN_POINT('',(-202.4825,-95.,9.));
#13193=CARTESIAN_POINT('Ctrl Pts',(-202.486523858474,-95.0002304794208,
3.88741669750803));
#13194=CARTESIAN_POINT('Ctrl Pts',(-202.486878246653,-94.5656573186005,
3.91478375102098));
#13195=CARTESIAN_POINT('Ctrl Pts',(-202.593838479751,-94.1309207445616,
3.94215080453392));
#13196=CARTESIAN_POINT('Ctrl Pts',(-202.80640573248,-93.7560710993726,3.96951785804687));
#13197=CARTESIAN_POINT('Ctrl Pts',(-203.217833592236,-93.0305426594524,
4.02248729764831));
#13198=CARTESIAN_POINT('Ctrl Pts',(-204.024889852448,-92.5293645510928,
4.07545673724974));
#13199=CARTESIAN_POINT('Ctrl Pts',(-204.8576244336,-92.4822740183969,4.12842617685117));
#13200=CARTESIAN_POINT('Ctrl Pts',(-205.690359014752,-92.435183485701,4.18139561645261));
#13201=CARTESIAN_POINT('Ctrl Pts',(-206.548771916843,-92.8421805286688,
4.23436505605405));
#13202=CARTESIAN_POINT('Ctrl Pts',(-207.0393714627,-93.5166999772584,4.28733449565548));
#13203=CARTESIAN_POINT('Ctrl Pts',(-207.529971008557,-94.1912194258479,
4.34030393525692));
#13204=CARTESIAN_POINT('Ctrl Pts',(-207.65275719818,-95.1332612800593,4.39327337485835));
#13205=CARTESIAN_POINT('Ctrl Pts',(-207.351445528426,-95.9109988184287,
4.44624281445978));
#13206=CARTESIAN_POINT('Ctrl Pts',(-207.050133858673,-96.688736356798,4.49921225406122));
#13207=CARTESIAN_POINT('Ctrl Pts',(-206.324724329544,-97.3021695793252,
4.55218169366266));
#13208=CARTESIAN_POINT('Ctrl Pts',(-205.507740615314,-97.4701041249105,
4.6051511332641));
#13209=CARTESIAN_POINT('Ctrl Pts',(-204.690756901084,-97.6380386704957,
4.65812057286553));
#13210=CARTESIAN_POINT('Ctrl Pts',(-203.782199001753,-97.3604745391391,
4.71109001246697));
#13211=CARTESIAN_POINT('Ctrl Pts',(-203.198544780993,-96.7646455775167,
4.7640594520684));
#13212=CARTESIAN_POINT('Ctrl Pts',(-202.745466065518,-96.3021158621945,
4.80517853388161));
#13213=CARTESIAN_POINT('Ctrl Pts',(-202.488177432177,-95.6477966985894,
4.84629761569482));
#13214=CARTESIAN_POINT('Ctrl Pts',(-202.482163763775,-94.997700765499,4.88741669750803));
#13215=CARTESIAN_POINT('Ctrl Pts',(-202.478335348143,-95.0004148939562,
4.61258330249195));
#13216=CARTESIAN_POINT('Ctrl Pts',(-202.478284511357,-95.0226822475079,
4.61116928343626));
#13217=CARTESIAN_POINT('Ctrl Pts',(-202.478553898799,-95.0449483397394,
4.60975526438057));
#13218=CARTESIAN_POINT('Ctrl Pts',(-202.479147281308,-95.0672057942804,
4.60834124532487));
#13219=CARTESIAN_POINT('Ctrl Pts',(-202.50137551002,-95.9009745396454,4.55537180572344));
#13220=CARTESIAN_POINT('Ctrl Pts',(-202.978255240917,-96.7226223010713,
4.502402366122));
#13221=CARTESIAN_POINT('Ctrl Pts',(-203.691187470346,-97.155510336405,4.44943292652057));
#13222=CARTESIAN_POINT('Ctrl Pts',(-204.404119699775,-97.5883983717386,
4.39646348691913));
#13223=CARTESIAN_POINT('Ctrl Pts',(-205.353104427737,-97.6325266809801,
4.34349404731769));
#13224=CARTESIAN_POINT('Ctrl Pts',(-206.103132358242,-97.2676670937981,
4.29052460771626));
#13225=CARTESIAN_POINT('Ctrl Pts',(-206.853160288746,-96.9028075066161,
4.23755516811482));
#13226=CARTESIAN_POINT('Ctrl Pts',(-207.404231421792,-96.1289600230108,
4.18458572851339));
#13227=CARTESIAN_POINT('Ctrl Pts',(-207.503737829587,-95.3008520048615,
4.13161628891195));
#13228=CARTESIAN_POINT('Ctrl Pts',(-207.603244237383,-94.4727439867123,
4.07864684931052));
#13229=CARTESIAN_POINT('Ctrl Pts',(-207.251185919929,-93.5903754340193,
4.02567740970908));
#13230=CARTESIAN_POINT('Ctrl Pts',(-206.60894444252,-93.058219160391,3.97270797010765));
#13231=CARTESIAN_POINT('Ctrl Pts',(-205.966702965111,-92.5260628867627,
3.91973853050621));
#13232=CARTESIAN_POINT('Ctrl Pts',(-205.034278327748,-92.3441188921993,
3.86676909090478));
#13233=CARTESIAN_POINT('Ctrl Pts',(-204.239088773406,-92.5957892868688,
3.81379965130334));
#13234=CARTESIAN_POINT('Ctrl Pts',(-203.443899219063,-92.8474596815382,
3.7608302117019));
#13235=CARTESIAN_POINT('Ctrl Pts',(-202.78594474774,-93.5327444654406,3.70786077210047));
#13236=CARTESIAN_POINT('Ctrl Pts',(-202.566828012252,-94.3375129236185,
3.65489133249903));
#13237=CARTESIAN_POINT('Ctrl Pts',(-202.508489987599,-94.5517758919359,
3.64078865583001));
#13238=CARTESIAN_POINT('Ctrl Pts',(-202.481258832434,-94.7745084214562,
3.62668597916098));
#13239=CARTESIAN_POINT('Ctrl Pts',(-202.483233733754,-94.9977147790846,
3.61258330249195));
#13240=CARTESIAN_POINT('Origin',(-205.,-95.,9.));
#13241=CARTESIAN_POINT('',(-202.486303966252,-95.0008035932749,2.61258330249195));
#13242=CARTESIAN_POINT('',(-202.481315987002,-95.0021961802459,2.88741669750803));
#13243=CARTESIAN_POINT('',(-202.4825,-95.,9.));
#13244=CARTESIAN_POINT('Ctrl Pts',(-202.481315987002,-95.0021961802459,
2.88741669750803));
#13245=CARTESIAN_POINT('Ctrl Pts',(-202.487520204672,-94.3247868793523,
2.9303004467457));
#13246=CARTESIAN_POINT('Ctrl Pts',(-202.769924023565,-93.6428175431098,
2.97318419598336));
#13247=CARTESIAN_POINT('Ctrl Pts',(-203.258228221064,-93.1764194592973,
3.01606794522103));
#13248=CARTESIAN_POINT('Ctrl Pts',(-203.861375104355,-92.6003307177601,
3.06903738482246));
#13249=CARTESIAN_POINT('Ctrl Pts',(-204.778661384897,-92.353136093667,3.1220068244239));
#13250=CARTESIAN_POINT('Ctrl Pts',(-205.589608158919,-92.5481482223093,
3.17497626402534));
#13251=CARTESIAN_POINT('Ctrl Pts',(-206.400554932941,-92.7431603509516,
3.22794570362677));
#13252=CARTESIAN_POINT('Ctrl Pts',(-207.105162200444,-93.3803792323294,
3.28091514322821));
#13253=CARTESIAN_POINT('Ctrl Pts',(-207.380441927112,-94.1677072917534,
3.33388458282964));
#13254=CARTESIAN_POINT('Ctrl Pts',(-207.655721653779,-94.9550353511775,
3.38685402243108));
#13255=CARTESIAN_POINT('Ctrl Pts',(-207.50167383961,-95.8924725886478,3.43982346203251));
#13256=CARTESIAN_POINT('Ctrl Pts',(-206.988913141991,-96.5503030135196,
3.49279290163395));
#13257=CARTESIAN_POINT('Ctrl Pts',(-206.476152444371,-97.2081334383915,
3.54576234123538));
#13258=CARTESIAN_POINT('Ctrl Pts',(-205.604678863301,-97.5863570506648,
3.59873178083682));
#13259=CARTESIAN_POINT('Ctrl Pts',(-204.773971018082,-97.5115982600209,
3.65170122043826));
#13260=CARTESIAN_POINT('Ctrl Pts',(-203.943263172863,-97.4368394693769,
3.70467066003969));
#13261=CARTESIAN_POINT('Ctrl Pts',(-203.153321063494,-96.9090982758155,
3.75764009964112));
#13262=CARTESIAN_POINT('Ctrl Pts',(-202.766249738459,-96.1702882932945,
3.81060953924256));
#13263=CARTESIAN_POINT('Ctrl Pts',(-202.57916168199,-95.8131899633733,3.83621192533105));
#13264=CARTESIAN_POINT('Ctrl Pts',(-202.486192321761,-95.4067817306088,
3.86181431141954));
#13265=CARTESIAN_POINT('Ctrl Pts',(-202.486523858474,-95.0002304794208,
3.88741669750803));
#13266=CARTESIAN_POINT('Ctrl Pts',(-202.483233733754,-94.9977147790846,
3.61258330249195));
#13267=CARTESIAN_POINT('Ctrl Pts',(-202.488676531827,-95.6128681141961,
3.57371653955955));
#13268=CARTESIAN_POINT('Ctrl Pts',(-202.715952540883,-96.2316203881349,
3.53484977662714));
#13269=CARTESIAN_POINT('Ctrl Pts',(-203.125272134475,-96.6865973078459,
3.49598301369473));
#13270=CARTESIAN_POINT('Ctrl Pts',(-203.683111991839,-97.3066611014422,
3.44301357409329));
#13271=CARTESIAN_POINT('Ctrl Pts',(-204.579070706222,-97.6225365561815,
3.39004413449185));
#13272=CARTESIAN_POINT('Ctrl Pts',(-205.402445810223,-97.4894281303028,
3.33707469489042));
#13273=CARTESIAN_POINT('Ctrl Pts',(-206.225820914224,-97.3563197044241,
3.28410525528898));
#13274=CARTESIAN_POINT('Ctrl Pts',(-206.976612407843,-96.7742273979274,
3.23113581568755));
#13275=CARTESIAN_POINT('Ctrl Pts',(-207.310661665506,-96.0099790681416,
3.17816637608611));
#13276=CARTESIAN_POINT('Ctrl Pts',(-207.644710923168,-95.2457307383558,
3.12519693648468));
#13277=CARTESIAN_POINT('Ctrl Pts',(-207.562017944873,-94.2993263852809,
3.07222749688324));
#13278=CARTESIAN_POINT('Ctrl Pts',(-207.100488731034,-93.6045924816996,
3.01925805728181));
#13279=CARTESIAN_POINT('Ctrl Pts',(-206.638959517195,-92.9098585781182,
2.96628861768037));
#13280=CARTESIAN_POINT('Ctrl Pts',(-205.798594067812,-92.4667951240303,
2.91331917807893));
#13281=CARTESIAN_POINT('Ctrl Pts',(-204.964611205932,-92.4784999179239,
2.8603497384775));
#13282=CARTESIAN_POINT('Ctrl Pts',(-204.130628344053,-92.4902047118176,
2.80738029887606));
#13283=CARTESIAN_POINT('Ctrl Pts',(-203.303028069677,-92.9566777536927,
2.75441085927463));
#13284=CARTESIAN_POINT('Ctrl Pts',(-202.861177729107,-93.6640904345609,
2.70144141967319));
#13285=CARTESIAN_POINT('Ctrl Pts',(-202.614104513341,-94.0596604044974,
2.67182204727945));
#13286=CARTESIAN_POINT('Ctrl Pts',(-202.487647821326,-94.5305675271913,
2.6422026748857));
#13287=CARTESIAN_POINT('Ctrl Pts',(-202.486303966252,-95.0008035932749,
2.61258330249195));
#13288=CARTESIAN_POINT('Origin',(-205.,-95.,9.));
#13289=CARTESIAN_POINT('',(-202.480282573446,-95.0019224211138,1.61258330249195));
#13290=CARTESIAN_POINT('',(-202.479323384637,-94.9985362448309,1.88741669750803));
#13291=CARTESIAN_POINT('',(-202.4825,-95.,9.));
#13292=CARTESIAN_POINT('Ctrl Pts',(-202.479323384637,-94.9985362448309,
1.88741669750803));
#13293=CARTESIAN_POINT('Ctrl Pts',(-202.478731654615,-94.9129221908085,
1.89284770286898));
#13294=CARTESIAN_POINT('Ctrl Pts',(-202.482714729456,-94.8273638427469,
1.89827870822993));
#13295=CARTESIAN_POINT('Ctrl Pts',(-202.49145403661,-94.7422941092908,1.90370971359088));
#13296=CARTESIAN_POINT('Ctrl Pts',(-202.576689857917,-93.912595773765,1.95667915319232));
#13297=CARTESIAN_POINT('Ctrl Pts',(-203.114357719001,-93.1293764342375,
2.00964859279375));
#13298=CARTESIAN_POINT('Ctrl Pts',(-203.857993504046,-92.7516592929174,
2.06261803239519));
#13299=CARTESIAN_POINT('Ctrl Pts',(-204.60162928909,-92.3739421515973,2.11558747199662));
#13300=CARTESIAN_POINT('Ctrl Pts',(-205.551232998096,-92.4017272084846,
2.16855691159806));
#13301=CARTESIAN_POINT('Ctrl Pts',(-206.271511681291,-92.8222780291104,
2.22152635119949));
#13302=CARTESIAN_POINT('Ctrl Pts',(-206.991790364487,-93.2428288497361,
2.27449579080093));
#13303=CARTESIAN_POINT('Ctrl Pts',(-207.482744021872,-94.0561454341005,
2.32746523040236));
#13304=CARTESIAN_POINT('Ctrl Pts',(-207.519322200074,-94.8894079662103,
2.3804346700038));
#13305=CARTESIAN_POINT('Ctrl Pts',(-207.555900378275,-95.7226704983201,
2.43340410960524));
#13306=CARTESIAN_POINT('Ctrl Pts',(-207.138103077293,-96.5758789781754,
2.48637354920667));
#13307=CARTESIAN_POINT('Ctrl Pts',(-206.457446264656,-97.0579274254718,
2.53934298880811));
#13308=CARTESIAN_POINT('Ctrl Pts',(-205.776789452019,-97.5399758727682,
2.59231242840954));
#13309=CARTESIAN_POINT('Ctrl Pts',(-204.833273127727,-97.6508642875058,
2.64528186801098));
#13310=CARTESIAN_POINT('Ctrl Pts',(-204.059399892623,-97.3397620309669,
2.69825130761241));
#13311=CARTESIAN_POINT('Ctrl Pts',(-203.28552665752,-97.028659774428,2.75122074721385));
#13312=CARTESIAN_POINT('Ctrl Pts',(-202.681296511605,-96.2955668466128,
2.80419018681529));
#13313=CARTESIAN_POINT('Ctrl Pts',(-202.523685181668,-95.4765289532145,
2.85715962641672));
#13314=CARTESIAN_POINT('Ctrl Pts',(-202.493675064825,-95.3205793594267,
2.86724531678049));
#13315=CARTESIAN_POINT('Ctrl Pts',(-202.479856837104,-95.1615138840336,
2.87733100714426));
#13316=CARTESIAN_POINT('Ctrl Pts',(-202.481315987002,-95.0021961802459,
2.88741669750803));
#13317=CARTESIAN_POINT('Ctrl Pts',(-202.486303966252,-95.0008035932749,
2.61258330249195));
#13318=CARTESIAN_POINT('Ctrl Pts',(-202.485244554665,-95.371508400945,2.58923323528426));
#13319=CARTESIAN_POINT('Ctrl Pts',(-202.561939805054,-95.7417961628412,
2.56588316807658));
#13320=CARTESIAN_POINT('Ctrl Pts',(-202.71859261042,-96.074427935554,2.54253310086889));
#13321=CARTESIAN_POINT('Ctrl Pts',(-203.073958239067,-96.8290004358175,
2.48956366126745));
#13322=CARTESIAN_POINT('Ctrl Pts',(-203.840789903126,-97.3897931164833,
2.43659422166602));
#13323=CARTESIAN_POINT('Ctrl Pts',(-204.667576276604,-97.4997418602453,
2.38362478206458));
#13324=CARTESIAN_POINT('Ctrl Pts',(-205.494362650082,-97.6096906040073,
2.33065534246314));
#13325=CARTESIAN_POINT('Ctrl Pts',(-206.38110373298,-97.2687954108656,2.27768590286171));
#13326=CARTESIAN_POINT('Ctrl Pts',(-206.921322319868,-96.6333204974726,
2.22471646326027));
#13327=CARTESIAN_POINT('Ctrl Pts',(-207.461540906757,-95.9978455840796,
2.17174702365884));
#13328=CARTESIAN_POINT('Ctrl Pts',(-207.655236997636,-95.0677909504354,
2.1187775840574));
#13329=CARTESIAN_POINT('Ctrl Pts',(-207.41362148715,-94.2694889285932,2.06580814445597));
#13330=CARTESIAN_POINT('Ctrl Pts',(-207.172005976663,-93.4711869067511,
2.01283870485453));
#13331=CARTESIAN_POINT('Ctrl Pts',(-206.495078864811,-92.8046374967111,
1.9598692652531));
#13332=CARTESIAN_POINT('Ctrl Pts',(-205.693139549457,-92.5753822193073,
1.90689982565166));
#13333=CARTESIAN_POINT('Ctrl Pts',(-204.891200234104,-92.3461269419034,
1.85393038605022));
#13334=CARTESIAN_POINT('Ctrl Pts',(-203.964248715248,-92.5541657971357,
1.80096094644879));
#13335=CARTESIAN_POINT('Ctrl Pts',(-203.337194817498,-93.1041370117052,
1.74799150684735));
#13336=CARTESIAN_POINT('Ctrl Pts',(-202.802872618589,-93.5727758795276,
1.70285543872889));
#13337=CARTESIAN_POINT('Ctrl Pts',(-202.48630621031,-94.2896919793449,1.65771937061042));
#13338=CARTESIAN_POINT('Ctrl Pts',(-202.480282573446,-95.0019224211138,
1.61258330249195));
#13339=CARTESIAN_POINT('Origin',(-205.,-95.,9.));
#13340=CARTESIAN_POINT('',(-202.480223490507,-94.9981350405341,0.612583302491955));
#13341=CARTESIAN_POINT('',(-202.485813979692,-94.9986458132734,0.887416697508031));
#13342=CARTESIAN_POINT('',(-202.4825,-95.,9.));
#13343=CARTESIAN_POINT('',(-206.913465996665,-93.3640127966251,0.));
#13344=CARTESIAN_POINT('Ctrl Pts',(-202.480223490507,-94.9981350405341,
0.612583302491955));
#13345=CARTESIAN_POINT('Ctrl Pts',(-202.486186751135,-95.7125466839347,
0.56729718713227));
#13346=CARTESIAN_POINT('Ctrl Pts',(-202.805062421801,-96.431520077419,0.522011071772584));
#13347=CARTESIAN_POINT('Ctrl Pts',(-203.34252319783,-96.9003741596628,0.476724956412899));
#13348=CARTESIAN_POINT('Ctrl Pts',(-203.971170541235,-97.4487748735251,
0.423755516811463));
#13349=CARTESIAN_POINT('Ctrl Pts',(-204.8988660792,-97.6549851699424,0.370786077210027));
#13350=CARTESIAN_POINT('Ctrl Pts',(-205.700052550654,-97.4230464763398,
0.317816637608592));
#13351=CARTESIAN_POINT('Ctrl Pts',(-206.501239022107,-97.1911077827372,
0.264847198007156));
#13352=CARTESIAN_POINT('Ctrl Pts',(-207.175916427048,-96.5210200991147,
0.21187775840572));
#13353=CARTESIAN_POINT('Ctrl Pts',(-207.41509417905,-95.7234547622828,0.158908318804285));
#13354=CARTESIAN_POINT('Ctrl Pts',(-207.654271931051,-94.9258894254509,
0.105938879202849));
#13355=CARTESIAN_POINT('Ctrl Pts',(-207.457950030113,-94.0008464354096,
0.052969439601414));
#13356=CARTESIAN_POINT('Ctrl Pts',(-206.913465996665,-93.3640127966251,
-2.14147317656561E-14));
#13357=CARTESIAN_POINT('',(-203.08284916835,-93.3612116138494,1.21293810816754E-15));
#13358=CARTESIAN_POINT('Origin',(-205.,-95.,0.));
#13359=CARTESIAN_POINT('Ctrl Pts',(-203.082846138209,-93.3612093103599,
7.63278329429795E-16));
#13360=CARTESIAN_POINT('Ctrl Pts',(-203.61481505219,-92.7406416726252,0.0519060689145028));
#13361=CARTESIAN_POINT('Ctrl Pts',(-204.477409065994,-92.4011123108223,
0.103812137829005));
#13362=CARTESIAN_POINT('Ctrl Pts',(-205.289479056896,-92.4950343384225,
0.155718206743507));
#13363=CARTESIAN_POINT('Ctrl Pts',(-206.118185472827,-92.5908804942238,
0.208687646344942));
#13364=CARTESIAN_POINT('Ctrl Pts',(-206.894276546249,-93.1381197102899,
0.261657085946378));
#13365=CARTESIAN_POINT('Ctrl Pts',(-207.262506848597,-93.886393298846,0.314626525547813));
#13366=CARTESIAN_POINT('Ctrl Pts',(-207.630737150946,-94.6346668874021,
0.367595965149249));
#13367=CARTESIAN_POINT('Ctrl Pts',(-207.591106682221,-95.5839748484483,
0.420565404750684));
#13368=CARTESIAN_POINT('Ctrl Pts',(-207.161534923276,-96.2989227744467,
0.47353484435212));
#13369=CARTESIAN_POINT('Ctrl Pts',(-206.73196316433,-97.0138707004452,0.526504283953556));
#13370=CARTESIAN_POINT('Ctrl Pts',(-205.912450115163,-97.4944585913958,
0.579473723554992));
#13371=CARTESIAN_POINT('Ctrl Pts',(-205.078775381405,-97.5205022929071,
0.632443163156427));
#13372=CARTESIAN_POINT('Ctrl Pts',(-204.245100647647,-97.5465459944184,
0.685412602757863));
#13373=CARTESIAN_POINT('Ctrl Pts',(-203.397264229298,-97.1180455064903,
0.738382042359298));
#13374=CARTESIAN_POINT('Ctrl Pts',(-202.92385184891,-96.4313676110377,0.791351481960734));
#13375=CARTESIAN_POINT('Ctrl Pts',(-202.637658761556,-96.0162486258607,
0.823373220476499));
#13376=CARTESIAN_POINT('Ctrl Pts',(-202.488302433328,-95.5067762975669,
0.855394958992265));
#13377=CARTESIAN_POINT('Ctrl Pts',(-202.485813979692,-94.9986458132734,
0.887416697508031));
#13378=CARTESIAN_POINT('Origin',(-205.,-95.,-2.20842344717744));
#13379=CARTESIAN_POINT('',(-201.921316222253,-94.9999604485794,16.2084234471775));
#13380=CARTESIAN_POINT('',(-201.931367503445,-94.9992219789103,16.2915765528226));
#13381=CARTESIAN_POINT('',(-201.9265,-94.9999999999997,-2.20842344717744));
#13382=CARTESIAN_POINT('',(-205.793799282533,-97.9692229537457,17.));
#13383=CARTESIAN_POINT('Ctrl Pts',(-201.931367503445,-94.9992219789103,
16.2915765528226));
#13384=CARTESIAN_POINT('Ctrl Pts',(-201.930437830903,-94.5288592028842,
16.315839943476));
#13385=CARTESIAN_POINT('Ctrl Pts',(-202.253352028229,-93.0329481124781,
16.3930727737308));
#13386=CARTESIAN_POINT('Ctrl Pts',(-204.582352673002,-91.390717466756,16.5232750435871));
#13387=CARTESIAN_POINT('Ctrl Pts',(-207.810248356741,-92.6929302430059,
16.6821833623914));
#13388=CARTESIAN_POINT('Ctrl Pts',(-208.456461600838,-96.1151764142335,
16.8410916811957));
#13389=CARTESIAN_POINT('Ctrl Pts',(-206.782006578242,-97.7050332130129,
16.9470305603986));
#13390=CARTESIAN_POINT('Ctrl Pts',(-205.793799282533,-97.9692229537457,
17.));
#13391=CARTESIAN_POINT('',(-204.206200717467,-97.9692229537457,17.));
#13392=CARTESIAN_POINT('Origin',(-205.,-95.,17.));
#13393=CARTESIAN_POINT('Ctrl Pts',(-201.921316222253,-94.9999604485793,
16.2084234471775));
#13394=CARTESIAN_POINT('Ctrl Pts',(-201.921316030809,-94.9985182315119,
16.2084984707981));
#13395=CARTESIAN_POINT('Ctrl Pts',(-201.921967711053,-93.9788178721187,
16.2615429340201));
#13396=CARTESIAN_POINT('Ctrl Pts',(-203.036133983161,-91.9425114866494,
16.3675568368436));
#13397=CARTESIAN_POINT('Ctrl Pts',(-206.506731020769,-91.6928976656653,
16.5264651556479));
#13398=CARTESIAN_POINT('Ctrl Pts',(-208.595808729299,-94.4759987242795,
16.6853734744522));
#13399=CARTESIAN_POINT('Ctrl Pts',(-207.396709451193,-97.716016535546,16.8432184225696));
#13400=CARTESIAN_POINT('Ctrl Pts',(-205.16879615822,-98.2310729989852,16.9480939310855));
#13401=CARTESIAN_POINT('Ctrl Pts',(-204.204429055805,-97.9745938792693,
17.));
#13402=CARTESIAN_POINT('Origin',(-205.,-95.,-2.20842344717744));
#13403=CARTESIAN_POINT('',(-201.928214488845,-94.9973269196036,15.2084234471775));
#13404=CARTESIAN_POINT('',(-201.926872790932,-95.0028204748396,15.2915765528226));
#13405=CARTESIAN_POINT('',(-201.9265,-94.9999999999997,-2.20842344717744));
#13406=CARTESIAN_POINT('Ctrl Pts',(-201.926872790932,-95.0028204748396,
15.2915765528226));
#13407=CARTESIAN_POINT('Ctrl Pts',(-201.933847540659,-94.2344924303963,
15.3313566392007));
#13408=CARTESIAN_POINT('Ctrl Pts',(-202.614657567475,-92.4320707201956,
15.4241061651802));
#13409=CARTESIAN_POINT('Ctrl Pts',(-205.641602982121,-91.4231516321926,
15.5698251307612));
#13410=CARTESIAN_POINT('Ctrl Pts',(-208.35434189336,-93.6020966294465,15.7287334495655));
#13411=CARTESIAN_POINT('Ctrl Pts',(-207.991790944675,-97.0626878467749,
15.8876417683698));
#13412=CARTESIAN_POINT('Ctrl Pts',(-204.886537405266,-98.6320975090182,
16.0465500871742));
#13413=CARTESIAN_POINT('Ctrl Pts',(-202.34331561747,-97.1406732810359,16.1811950153251));
#13414=CARTESIAN_POINT('Ctrl Pts',(-201.932467400235,-95.555708789217,16.2628705038745));
#13415=CARTESIAN_POINT('Ctrl Pts',(-201.931367503445,-94.9992219789103,
16.2915765528226));
#13416=CARTESIAN_POINT('Ctrl Pts',(-201.928214488845,-94.9973269196036,
15.2084234471775));
#13417=CARTESIAN_POINT('Ctrl Pts',(-201.925712567505,-94.6958484416858,
15.2240151665228));
#13418=CARTESIAN_POINT('Ctrl Pts',(-202.105035794616,-93.3730750516054,
15.2925763254696));
#13419=CARTESIAN_POINT('Ctrl Pts',(-204.001156151974,-91.5060233657571,
15.4141069240177));
#13420=CARTESIAN_POINT('Ctrl Pts',(-207.396173587353,-92.2679785768132,
15.5730152428221));
#13421=CARTESIAN_POINT('Ctrl Pts',(-208.594403743819,-95.5346307410897,
15.7319235616264));
#13422=CARTESIAN_POINT('Ctrl Pts',(-206.497329095757,-98.3111182304646,
15.8908318804307));
#13423=CARTESIAN_POINT('Ctrl Pts',(-203.02914899186,-98.0521756469229,16.0496651756144));
#13424=CARTESIAN_POINT('Ctrl Pts',(-201.921451197495,-96.0167766044663,
16.1555290311966));
#13425=CARTESIAN_POINT('Ctrl Pts',(-201.921316222253,-94.9999604485793,
16.2084234471775));
#13426=CARTESIAN_POINT('Origin',(-205.,-95.,-2.20842344717744));
#13427=CARTESIAN_POINT('',(-201.930806967845,-95.0014123568597,14.2084234471775));
#13428=CARTESIAN_POINT('',(-201.921581898641,-94.9991754600276,14.2915765528226));
#13429=CARTESIAN_POINT('',(-201.9265,-94.9999999999997,-2.20842344717744));
#13430=CARTESIAN_POINT('Ctrl Pts',(-201.921581898641,-94.9991754600276,
14.2915765528226));
#13431=CARTESIAN_POINT('Ctrl Pts',(-201.921422031341,-94.9544247205291,
14.293903895324));
#13432=CARTESIAN_POINT('Ctrl Pts',(-201.942596590982,-93.891318641259,14.3492006774268));
#13433=CARTESIAN_POINT('Ctrl Pts',(-203.167697451582,-91.8618096795541,
14.4574668991311));
#13434=CARTESIAN_POINT('Ctrl Pts',(-206.64568000845,-91.7600451831499,14.6163752179354));
#13435=CARTESIAN_POINT('Ctrl Pts',(-208.614921940056,-94.6286346539956,
14.7752835367397));
#13436=CARTESIAN_POINT('Ctrl Pts',(-207.270042986249,-97.8376885432202,
14.934191855544));
#13437=CARTESIAN_POINT('Ctrl Pts',(-203.844015760112,-98.4451795972611,
15.0931001743483));
#13438=CARTESIAN_POINT('Ctrl Pts',(-202.070126976119,-96.5327748382561,
15.2122284067745));
#13439=CARTESIAN_POINT('Ctrl Pts',(-201.924560266095,-95.2575647675798,
15.2783871995992));
#13440=CARTESIAN_POINT('Ctrl Pts',(-201.926872790932,-95.0028204748396,
15.2915765528226));
#13441=CARTESIAN_POINT('Ctrl Pts',(-201.930806967845,-95.0014123568597,
14.2084234471775));
#13442=CARTESIAN_POINT('Ctrl Pts',(-201.93330334053,-94.39862726836,14.2395318622475));
#13443=CARTESIAN_POINT('Ctrl Pts',(-202.396531719082,-92.765916828767,14.323609716919));
#13444=CARTESIAN_POINT('Ctrl Pts',(-205.050996758677,-91.3664108756636,
14.4606570111919));
#13445=CARTESIAN_POINT('Ctrl Pts',(-208.082134098584,-93.0748973262563,
14.6195653299962));
#13446=CARTESIAN_POINT('Ctrl Pts',(-208.287605318196,-96.548296522874,14.7784736488005));
#13447=CARTESIAN_POINT('Ctrl Pts',(-205.479036782975,-98.6022345010335,
14.9373819676048));
#13448=CARTESIAN_POINT('Ctrl Pts',(-202.549953768568,-97.4761895493396,
15.0806985670638));
#13449=CARTESIAN_POINT('Ctrl Pts',(-201.934212295366,-95.7200553090311,
15.1710457269214));
#13450=CARTESIAN_POINT('Ctrl Pts',(-201.928214488845,-94.9973269196036,
15.2084234471775));
#13451=CARTESIAN_POINT('Origin',(-205.,-95.,-2.20842344717744));
#13452=CARTESIAN_POINT('',(-201.923037944235,-95.0020215915549,13.2084234471775));
#13453=CARTESIAN_POINT('',(-201.929332692288,-94.9976509811143,13.2915765528226));
#13454=CARTESIAN_POINT('',(-201.9265,-94.9999999999997,-2.20842344717744));
#13455=CARTESIAN_POINT('Ctrl Pts',(-201.929332692288,-94.9976509811143,
13.2915765528226));
#13456=CARTESIAN_POINT('Ctrl Pts',(-201.926879286391,-94.6523048684722,
13.3094205910487));
#13457=CARTESIAN_POINT('Ctrl Pts',(-202.14011741618,-93.2847511636649,13.3802340688763));
#13458=CARTESIAN_POINT('Ctrl Pts',(-204.150349485118,-91.4667769681704,
13.5040169863052));
#13459=CARTESIAN_POINT('Ctrl Pts',(-207.509967453225,-92.3721426302753,
13.6629253051096));
#13460=CARTESIAN_POINT('Ctrl Pts',(-208.568475318891,-95.6866985528482,
13.8218336239139));
#13461=CARTESIAN_POINT('Ctrl Pts',(-206.355444885374,-98.3716969277542,
13.9807419427182));
#13462=CARTESIAN_POINT('Ctrl Pts',(-202.950369121919,-97.9715094124519,
14.1373229190211));
#13463=CARTESIAN_POINT('Ctrl Pts',(-201.925060550926,-95.9729347127417,
14.2409344557225));
#13464=CARTESIAN_POINT('Ctrl Pts',(-201.921581898641,-94.9991754600276,
14.2915765528226));
#13465=CARTESIAN_POINT('Ctrl Pts',(-201.923037944235,-95.0020215915549,
13.2084234471775));
#13466=CARTESIAN_POINT('Ctrl Pts',(-201.929861116958,-94.1043808714426,
13.2550485579722));
#13467=CARTESIAN_POINT('Ctrl Pts',(-202.817787000569,-92.1752061029806,
13.3546431083684));
#13468=CARTESIAN_POINT('Ctrl Pts',(-206.096505523284,-91.5354298452884,
13.5072070983661));
#13469=CARTESIAN_POINT('Ctrl Pts',(-208.506304586591,-94.045327873685,13.6661154171704));
#13470=CARTESIAN_POINT('Ctrl Pts',(-207.701562793806,-97.4304586389942,
13.8250237359747));
#13471=CARTESIAN_POINT('Ctrl Pts',(-204.420058427186,-98.5873720853337,
13.983932054779));
#13472=CARTESIAN_POINT('Ctrl Pts',(-202.208551898768,-96.8727802886784,
14.1117319585132));
#13473=CARTESIAN_POINT('Ctrl Pts',(-201.929052675175,-95.4250115526778,
14.1865624226461));
#13474=CARTESIAN_POINT('Ctrl Pts',(-201.930806967845,-95.0014123568597,
14.2084234471775));
#13475=CARTESIAN_POINT('Origin',(-205.,-95.,-2.20842344717744));
#13476=CARTESIAN_POINT('',(-201.924530264077,-94.9974318186093,12.2084234471775));
#13477=CARTESIAN_POINT('',(-201.930073780141,-95.0019865806918,12.2915765528226));
#13478=CARTESIAN_POINT('',(-201.9265,-94.9999999999997,-2.20842344717744));
#13479=CARTESIAN_POINT('Ctrl Pts',(-201.930073780141,-95.0019865806918,
12.2915765528226));
#13480=CARTESIAN_POINT('Ctrl Pts',(-201.933893603562,-94.3559450496333,
12.3249372867734));
#13481=CARTESIAN_POINT('Ctrl Pts',(-202.4491356456,-92.6785603743455,12.4112674603257));
#13482=CARTESIAN_POINT('Ctrl Pts',(-205.205169266307,-91.3718494299793,
12.5505670734794));
#13483=CARTESIAN_POINT('Ctrl Pts',(-208.161062939416,-93.2074453761791,
12.7094753922837));
#13484=CARTESIAN_POINT('Ctrl Pts',(-208.218929440283,-96.6864353664204,
12.868383711088));
#13485=CARTESIAN_POINT('Ctrl Pts',(-205.325717407468,-98.6193202618013,
13.0272920298923));
#13486=CARTESIAN_POINT('Ctrl Pts',(-202.49230593161,-97.3896064222378,13.1683563104705));
#13487=CARTESIAN_POINT('Ctrl Pts',(-201.93416214097,-95.6774534264036,13.2564511514473));
#13488=CARTESIAN_POINT('Ctrl Pts',(-201.929332692288,-94.9976509811143,
13.2915765528226));
#13489=CARTESIAN_POINT('Ctrl Pts',(-201.924530264077,-94.9974318186092,
12.2084234471775));
#13490=CARTESIAN_POINT('Ctrl Pts',(-201.922946574968,-94.8206195588585,
12.2175958140955));
#13491=CARTESIAN_POINT('Ctrl Pts',(-202.017340558395,-93.6244254438343,
12.279737620615));
#13492=CARTESIAN_POINT('Ctrl Pts',(-203.58671258731,-91.6521365902563,12.3948488667359));
#13493=CARTESIAN_POINT('Ctrl Pts',(-207.048879196816,-91.9987228122024,
12.5537571855402));
#13494=CARTESIAN_POINT('Ctrl Pts',(-208.632656258583,-95.0968464152565,
12.7126655043445));
#13495=CARTESIAN_POINT('Ctrl Pts',(-206.886054663924,-98.1061823072572,
12.8715738231488));
#13496=CARTESIAN_POINT('Ctrl Pts',(-203.410339233432,-98.2678049770775,
13.0304821419532));
#13497=CARTESIAN_POINT('Ctrl Pts',(-201.984203605419,-96.2651388949014,
13.1427653499627));
#13498=CARTESIAN_POINT('Ctrl Pts',(-201.922109507808,-95.1241645265866,
13.2020791183708));
#13499=CARTESIAN_POINT('Ctrl Pts',(-201.923037944235,-95.0020215915549,
13.2084234471775));
#13500=CARTESIAN_POINT('Origin',(-205.,-95.,-2.20842344717744));
#13501=CARTESIAN_POINT('',(-201.93133959706,-94.9994302440671,11.2084234471775));
#13502=CARTESIAN_POINT('',(-201.922093677493,-95.0013994409948,11.2915765528226));
#13503=CARTESIAN_POINT('',(-201.9265,-94.9999999999997,-2.20842344717744));
#13504=CARTESIAN_POINT('Ctrl Pts',(-201.922093677493,-95.0013994409948,
11.2915765528226));
#13505=CARTESIAN_POINT('Ctrl Pts',(-201.927419125191,-94.061156157063,11.3404539824981));
#13506=CARTESIAN_POINT('Ctrl Pts',(-202.890883202837,-92.0925151635822,
11.4423008517751));
#13507=CARTESIAN_POINT('Ctrl Pts',(-206.242562362063,-91.5850900798271,
11.5971171606536));
#13508=CARTESIAN_POINT('Ctrl Pts',(-208.54366376786,-94.1950042938844,11.7560254794579));
#13509=CARTESIAN_POINT('Ctrl Pts',(-207.595973838081,-97.542929574037,11.9149337982622));
#13510=CARTESIAN_POINT('Ctrl Pts',(-204.26832410821,-98.5595254425124,12.0738421170665));
#13511=CARTESIAN_POINT('Ctrl Pts',(-202.16923931098,-96.7844614271993,12.19938970192));
#13512=CARTESIAN_POINT('Ctrl Pts',(-201.927828571951,-95.3817155830347,
12.271967847172));
#13513=CARTESIAN_POINT('Ctrl Pts',(-201.930073780141,-95.0019865806918,
12.2915765528226));
#13514=CARTESIAN_POINT('Ctrl Pts',(-201.93133959706,-94.9994302440671,11.2084234471775));
#13515=CARTESIAN_POINT('Ctrl Pts',(-201.930548213561,-94.5208250022373,
11.2331125098202));
#13516=CARTESIAN_POINT('Ctrl Pts',(-202.261412933308,-93.0164261928261,
11.3107710120644));
#13517=CARTESIAN_POINT('Ctrl Pts',(-204.612024659808,-91.3868233012261,
11.4413989539101));
#13518=CARTESIAN_POINT('Ctrl Pts',(-207.827224979576,-92.7169385387114,
11.6003072727144));
#13519=CARTESIAN_POINT('Ctrl Pts',(-208.450457037378,-96.1401390066001,
11.7592155915187));
#13520=CARTESIAN_POINT('Ctrl Pts',(-205.910348648356,-98.5180727763361,
11.918123910323));
#13521=CARTESIAN_POINT('Ctrl Pts',(-202.730434611476,-97.7195893976379,
12.0678598622093));
#13522=CARTESIAN_POINT('Ctrl Pts',(-201.932092210478,-95.8416914803529,
12.1646263744941));
#13523=CARTESIAN_POINT('Ctrl Pts',(-201.924530264077,-94.9974318186092,
12.2084234471775));
#13524=CARTESIAN_POINT('Origin',(-205.,-95.,-2.20842344717744));
#13525=CARTESIAN_POINT('',(-201.926625204813,-95.0028238958017,10.2084234471775));
#13526=CARTESIAN_POINT('',(-201.925838838714,-94.9972120666634,10.2915765528226));
#13527=CARTESIAN_POINT('',(-201.9265,-94.9999999999997,-2.20842344717744));
#13528=CARTESIAN_POINT('Ctrl Pts',(-201.925838838714,-94.9972120666634,
10.2915765528226));
#13529=CARTESIAN_POINT('Ctrl Pts',(-201.923796651544,-94.7767411547191,
10.3030012386214));
#13530=CARTESIAN_POINT('Ctrl Pts',(-202.046093670253,-93.536326186288,10.3673953640217));
#13531=CARTESIAN_POINT('Ctrl Pts',(-203.730077621707,-91.5951698809454,
10.4847589290234));
#13532=CARTESIAN_POINT('Ctrl Pts',(-207.174414580991,-92.0883866643241,
10.6436672478277));
#13533=CARTESIAN_POINT('Ctrl Pts',(-208.625272555405,-95.2509380113502,
10.802575566632));
#13534=CARTESIAN_POINT('Ctrl Pts',(-206.752521169945,-98.1834321942526,
10.9614838854363));
#13535=CARTESIAN_POINT('Ctrl Pts',(-203.273077963447,-98.1973913220278,
11.1203922042406));
#13536=CARTESIAN_POINT('Ctrl Pts',(-201.960101924826,-96.1773510717403,
11.2304230933694));
#13537=CARTESIAN_POINT('Ctrl Pts',(-201.921647831937,-95.0801164454715,
11.2874845428967));
#13538=CARTESIAN_POINT('Ctrl Pts',(-201.922093677493,-95.0013994409948,
11.2915765528226));
#13539=CARTESIAN_POINT('Ctrl Pts',(-201.926625204813,-95.0028238958017,
10.2084234471775));
#13540=CARTESIAN_POINT('Ctrl Pts',(-201.93373191466,-94.2264345369936,10.248629205545));
#13541=CARTESIAN_POINT('Ctrl Pts',(-202.626469630616,-92.4158935511655,
10.3418044035139));
#13542=CARTESIAN_POINT('Ctrl Pts',(-205.670290617637,-91.4284063488314,
10.4879490410842));
#13543=CARTESIAN_POINT('Ctrl Pts',(-208.365431665519,-93.6290731507911,
10.6468573598885));
#13544=CARTESIAN_POINT('Ctrl Pts',(-207.975182577187,-97.0865903655397,
10.8057656786929));
#13545=CARTESIAN_POINT('Ctrl Pts',(-204.85731935509,-98.6311448545504,10.9646739974972));
#13546=CARTESIAN_POINT('Ctrl Pts',(-202.334353092009,-97.1239486684601,
11.0988932536587));
#13547=CARTESIAN_POINT('Ctrl Pts',(-201.932246096589,-95.5476542430574,
11.1801430702188));
#13548=CARTESIAN_POINT('Ctrl Pts',(-201.93133959706,-94.9994302440671,11.2084234471775));
#13549=CARTESIAN_POINT('Origin',(-205.,-95.,-2.20842344717744));
#13550=CARTESIAN_POINT('',(-201.921683699254,-94.9990313104991,9.20842344717747));
#13551=CARTESIAN_POINT('',(-201.931429552667,-95.000145803808,9.29157655282255));
#13552=CARTESIAN_POINT('',(-201.9265,-94.9999999999997,-2.20842344717744));
#13553=CARTESIAN_POINT('Ctrl Pts',(-201.931429552667,-95.000145803808,9.29157655282255));
#13554=CARTESIAN_POINT('Ctrl Pts',(-201.931650187457,-94.4778404498504,
9.31851793434612));
#13555=CARTESIAN_POINT('Ctrl Pts',(-202.306382510376,-92.9283336853723,
9.39842875547113));
#13556=CARTESIAN_POINT('Ctrl Pts',(-204.765726357252,-91.3736124246263,
9.53130901619759));
#13557=CARTESIAN_POINT('Ctrl Pts',(-207.921576173118,-92.8389901316329,
9.69021733500189));
#13558=CARTESIAN_POINT('Ctrl Pts',(-208.398957607323,-96.2855575327979,
9.84912565380619));
#13559=CARTESIAN_POINT('Ctrl Pts',(-205.76021269658,-98.5535401563045,10.0080339726105));
#13560=CARTESIAN_POINT('Ctrl Pts',(-202.664332808566,-97.6348429287674,
10.155517605616));
#13561=CARTESIAN_POINT('Ctrl Pts',(-201.933265052849,-95.798932999617,10.25003179902));
#13562=CARTESIAN_POINT('Ctrl Pts',(-201.925838838714,-94.9972120666634,
10.2915765528226));
#13563=CARTESIAN_POINT('Ctrl Pts',(-201.921683699254,-94.9990313104991,
9.20842344717747));
#13564=CARTESIAN_POINT('Ctrl Pts',(-201.921465341112,-94.9460909713989,
9.21117646166824));
#13565=CARTESIAN_POINT('Ctrl Pts',(-201.946710084923,-93.8747633774113,
9.26689891576045));
#13566=CARTESIAN_POINT('Ctrl Pts',(-203.192936111301,-91.8472090422419,
9.3755908094541));
#13567=CARTESIAN_POINT('Ctrl Pts',(-206.671623368988,-91.7733537483301,
9.53449912825839));
#13568=CARTESIAN_POINT('Ctrl Pts',(-208.617785005374,-94.6576516743914,
9.69340744706271));
#13569=CARTESIAN_POINT('Ctrl Pts',(-207.247201784069,-97.8558107190141,
9.85231576586701));
#13570=CARTESIAN_POINT('Ctrl Pts',(-203.816409083639,-98.4357944152506,
10.0112240846713));
#13571=CARTESIAN_POINT('Ctrl Pts',(-202.064207659429,-96.5161000870413,
10.1299266451081));
#13572=CARTESIAN_POINT('Ctrl Pts',(-201.924369115566,-95.2492957120694,
10.1956597659435));
#13573=CARTESIAN_POINT('Ctrl Pts',(-201.926625204813,-95.0028238958017,
10.2084234471775));
#13574=CARTESIAN_POINT('Origin',(-205.,-95.,-2.20842344717744));
#13575=CARTESIAN_POINT('',(-201.929523551853,-94.9977303344825,8.20842344717746));
#13576=CARTESIAN_POINT('',(-201.925302479416,-95.0027227980173,8.29157655282255));
#13577=CARTESIAN_POINT('',(-201.9265,-94.9999999999997,-2.20842344717744));
#13578=CARTESIAN_POINT('Ctrl Pts',(-201.925302479416,-95.0027227980173,
8.29157655282255));
#13579=CARTESIAN_POINT('Ctrl Pts',(-201.93285017436,-94.1837439219852,8.33403463007085));
#13580=CARTESIAN_POINT('Ctrl Pts',(-202.690770472001,-92.3306976061766,
8.42946214692058));
#13581=CARTESIAN_POINT('Ctrl Pts',(-205.821273849133,-91.4600734116028,
8.57785910337174));
#13582=CARTESIAN_POINT('Ctrl Pts',(-208.420584658025,-93.7731456550212,
8.73676742217605));
#13583=CARTESIAN_POINT('Ctrl Pts',(-207.883941683608,-97.2109842496187,
8.89567574098036));
#13584=CARTESIAN_POINT('Ctrl Pts',(-204.703333206878,-98.6218171958797,
9.05458405978466));
#13585=CARTESIAN_POINT('Ctrl Pts',(-202.287835459144,-97.0359644386318,
9.1865509970654));
#13586=CARTESIAN_POINT('Ctrl Pts',(-201.931216397484,-95.5047448005331,
9.26554849474469));
#13587=CARTESIAN_POINT('Ctrl Pts',(-201.931429552667,-95.000145803808,9.29157655282255));
#13588=CARTESIAN_POINT('Ctrl Pts',(-201.929523551853,-94.9977303344825,
8.20842344717746));
#13589=CARTESIAN_POINT('Ctrl Pts',(-201.927106317664,-94.6440906524844,
8.22669315739296));
#13590=CARTESIAN_POINT('Ctrl Pts',(-202.147009202964,-93.2680558099108,
8.29793230720989));
#13591=CARTESIAN_POINT('Ctrl Pts',(-204.178726159118,-91.4600734471682,
8.42214089662825));
#13592=CARTESIAN_POINT('Ctrl Pts',(-207.530971620008,-92.3923663255981,
8.58104921543255));
#13593=CARTESIAN_POINT('Ctrl Pts',(-208.562850587821,-95.7153086117373,
8.73995753423687));
#13594=CARTESIAN_POINT('Ctrl Pts',(-206.328347957964,-98.382463957492,8.89886585304117));
#13595=CARTESIAN_POINT('Ctrl Pts',(-202.935840595157,-97.9561304030613,
9.05502115735471));
#13596=CARTESIAN_POINT('Ctrl Pts',(-201.925666666051,-95.9646908021815,
9.1582070220668));
#13597=CARTESIAN_POINT('Ctrl Pts',(-201.921683699254,-94.9990313104991,
9.20842344717747));
#13598=CARTESIAN_POINT('Origin',(-205.,-95.,-2.20842344717744));
#13599=CARTESIAN_POINT('',(-201.929907480782,-95.0020818313008,7.20842344717746));
#13600=CARTESIAN_POINT('',(-201.922442534737,-94.9983308996675,7.29157655282255));
#13601=CARTESIAN_POINT('',(-201.9265,-94.9999999999997,-2.20842344717744));
#13602=CARTESIAN_POINT('Ctrl Pts',(-201.922442534737,-94.9983308996675,
7.29157655282255));
#13603=CARTESIAN_POINT('Ctrl Pts',(-201.921812073097,-94.902015678895,7.29658188619413));
#13604=CARTESIAN_POINT('Ctrl Pts',(-201.969634830997,-93.7870693467852,
7.35455665916715));
#13605=CARTESIAN_POINT('Ctrl Pts',(-203.328376614218,-91.7733537159122,
7.46550087174159));
#13606=CARTESIAN_POINT('Ctrl Pts',(-206.807063906854,-91.847209010566,7.62440919054591));
#13607=CARTESIAN_POINT('Ctrl Pts',(-208.629055206866,-94.8115078462396,
7.7833175093502));
#13608=CARTESIAN_POINT('Ctrl Pts',(-207.123969254423,-97.9486141817431,
7.94222582815452));
#13609=CARTESIAN_POINT('Ctrl Pts',(-203.67165202869,-98.3824639914755,8.10113414695881));
#13610=CARTESIAN_POINT('Ctrl Pts',(-202.034177190516,-96.4279351805356,
8.21758438851483));
#13611=CARTESIAN_POINT('Ctrl Pts',(-201.923433893705,-95.2054777102381,
8.28106519046941));
#13612=CARTESIAN_POINT('Ctrl Pts',(-201.925302479416,-95.0027227980173,
8.29157655282255));
#13613=CARTESIAN_POINT('Ctrl Pts',(-201.929907480782,-95.0020818313008,
7.20842344717746));
#13614=CARTESIAN_POINT('Ctrl Pts',(-201.933975214882,-94.3478859808551,
7.24220985311768));
#13615=CARTESIAN_POINT('Ctrl Pts',(-202.459390523649,-92.662093249463,7.32896569865933));
#13616=CARTESIAN_POINT('Ctrl Pts',(-205.234273640395,-91.3736124610605,
7.46869098380241));
#13617=CARTESIAN_POINT('Ctrl Pts',(-208.175343969469,-93.2328663330924,
7.62759930260672));
#13618=CARTESIAN_POINT('Ctrl Pts',(-208.205294437497,-96.7122086000577,
7.78650762141102));
#13619=CARTESIAN_POINT('Ctrl Pts',(-205.296666790141,-98.6218171594914,
7.94541594021533));
#13620=CARTESIAN_POINT('Ctrl Pts',(-202.481733314634,-97.3731878742982,
8.08605454880414));
#13621=CARTESIAN_POINT('Ctrl Pts',(-201.934114613849,-95.6693995137262,
8.17372371779152));
#13622=CARTESIAN_POINT('Ctrl Pts',(-201.929523551853,-94.9977303344825,
8.20842344717746));
#13623=CARTESIAN_POINT('Origin',(-205.,-95.,-2.20842344717744));
#13624=CARTESIAN_POINT('',(-201.921949435201,-95.0012666709355,6.20842344717746));
#13625=CARTESIAN_POINT('',(-201.930401808297,-94.9982329210887,6.29157655282255));
#13626=CARTESIAN_POINT('',(-201.9265,-94.9999999999997,-2.20842344717744));
#13627=CARTESIAN_POINT('Ctrl Pts',(-201.930401808297,-94.9982329210887,
6.29157655282255));
#13628=CARTESIAN_POINT('Ctrl Pts',(-201.928325217551,-94.6007106472249,
6.31209858191885));
#13629=CARTESIAN_POINT('Ctrl Pts',(-202.184887815006,-93.1797200737991,
6.38559005061659));
#13630=CARTESIAN_POINT('Ctrl Pts',(-204.329709375628,-91.4284063129477,
6.51205095891576));
#13631=CARTESIAN_POINT('Ctrl Pts',(-207.639365403312,-92.5021366622034,
6.67095927772007));
#13632=CARTESIAN_POINT('Ctrl Pts',(-208.529280728881,-95.8658802014486,
6.82986759652437));
#13633=CARTESIAN_POINT('Ctrl Pts',(-206.183590928253,-98.4357944497699,
6.98877591532868));
#13634=CARTESIAN_POINT('Ctrl Pts',(-202.860862148067,-97.8740792172285,
7.1426789007614));
#13635=CARTESIAN_POINT('Ctrl Pts',(-201.928483996284,-95.9212811085216,
7.2436124465927));
#13636=CARTESIAN_POINT('Ctrl Pts',(-201.922442534737,-94.9983308996675,
7.29157655282255));
#13637=CARTESIAN_POINT('Ctrl Pts',(-201.921949435201,-95.0012666709355,
6.20842344717746));
#13638=CARTESIAN_POINT('Ctrl Pts',(-201.926887034891,-94.0529526670259,
6.2577265488424));
#13639=CARTESIAN_POINT('Ctrl Pts',(-202.905053295201,-92.0770071799099,
6.35999909010877));
#13640=CARTESIAN_POINT('Ctrl Pts',(-206.269922365534,-91.5951699151535,
6.51524107097657));
#13641=CARTESIAN_POINT('Ctrl Pts',(-208.550008659151,-94.2234633034355,
6.67414938978088));
#13642=CARTESIAN_POINT('Ctrl Pts',(-207.575486691771,-97.5636768559377,
6.83305770858518));
#13643=CARTESIAN_POINT('Ctrl Pts',(-204.239787311058,-98.5535401206023,
6.9919660273895));
#13644=CARTESIAN_POINT('Ctrl Pts',(-202.162081059052,-96.7677662638285,
7.11708794025358));
#13645=CARTESIAN_POINT('Ctrl Pts',(-201.927597928226,-95.3735170482439,
7.18924041351624));
#13646=CARTESIAN_POINT('Ctrl Pts',(-201.929907480782,-95.0020818313008,
7.20842344717746));
#13647=CARTESIAN_POINT('Origin',(-205.,-95.,-2.20842344717744));
#13648=CARTESIAN_POINT('',(-201.926089504652,-94.997192970312,5.20842344717746));
#13649=CARTESIAN_POINT('',(-201.928899855331,-95.0025004707799,5.29157655282255));
#13650=CARTESIAN_POINT('',(-201.9265,-94.9999999999997,-2.20842344717744));
#13651=CARTESIAN_POINT('Ctrl Pts',(-201.928899855331,-95.0025004707799,
5.29157655282255));
#13652=CARTESIAN_POINT('Ctrl Pts',(-201.934224625714,-94.3052696210272,
5.32761527764357));
#13653=CARTESIAN_POINT('Ctrl Pts',(-202.515335032503,-92.5752228264589,
5.41662344206603));
#13654=CARTESIAN_POINT('Ctrl Pts',(-205.38797534409,-91.3868232649246,5.55860104608991));
#13655=CARTESIAN_POINT('Ctrl Pts',(-208.247484237019,-93.3692280610634,
5.71750936489423));
#13656=CARTESIAN_POINT('Ctrl Pts',(-208.129735877909,-96.8467063440184,
5.87641768369853));
#13657=CARTESIAN_POINT('Ctrl Pts',(-205.142680646343,-98.6311448910324,
6.03532600250284));
#13658=CARTESIAN_POINT('Ctrl Pts',(-202.427470198555,-97.2860600726802,
6.17371229221084));
#13659=CARTESIAN_POINT('Ctrl Pts',(-201.933685108993,-95.6267559752403,
6.25912914231742));
#13660=CARTESIAN_POINT('Ctrl Pts',(-201.930401808297,-94.9982329210887,
6.29157655282255));
#13661=CARTESIAN_POINT('Ctrl Pts',(-201.926089504652,-94.997192970312,5.20842344717746));
#13662=CARTESIAN_POINT('Ctrl Pts',(-201.9239736235,-94.7684597513135,5.22027380496568));
#13663=CARTESIAN_POINT('Ctrl Pts',(-202.051768758167,-93.5196634776365,
5.28509360235533));
#13664=CARTESIAN_POINT('Ctrl Pts',(-203.75743765042,-91.5850901141365,5.40288283934643));
#13665=CARTESIAN_POINT('Ctrl Pts',(-207.19770630733,-92.1059271419192,5.56179115815073));
#13666=CARTESIAN_POINT('Ctrl Pts',(-208.623142384989,-95.2800178195362,
5.72069947695504));
#13667=CARTESIAN_POINT('Ctrl Pts',(-206.726922019203,-98.1973912899037,
5.87960779575934));
#13668=CARTESIAN_POINT('Ctrl Pts',(-203.247478847662,-98.1834321622689,
6.03851611456366));
#13669=CARTESIAN_POINT('Ctrl Pts',(-201.955769755693,-96.1607774588135,
6.14812133170303));
#13670=CARTESIAN_POINT('Ctrl Pts',(-201.921582259335,-95.0717863642375,
6.20475710924096));
#13671=CARTESIAN_POINT('Ctrl Pts',(-201.921949435201,-95.0012666709355,
6.20842344717746));
#13672=CARTESIAN_POINT('Origin',(-205.,-95.,-2.20842344717744));
#13673=CARTESIAN_POINT('',(-201.931412543801,-95.0002813817275,4.20842344717746));
#13674=CARTESIAN_POINT('',(-201.921415568031,-95.0005065249549,4.29157655282255));
#13675=CARTESIAN_POINT('',(-201.9265,-94.9999999999997,-2.20842344717744));
#13676=CARTESIAN_POINT('Ctrl Pts',(-201.921415568031,-95.0005065249549,
4.29157655282255));
#13677=CARTESIAN_POINT('Ctrl Pts',(-201.923678444759,-94.0093290712259,
4.34313197336829));
#13678=CARTESIAN_POINT('Ctrl Pts',(-202.981928292525,-91.9956387425796,
4.44765683351546));
#13679=CARTESIAN_POINT('Ctrl Pts',(-206.413287426889,-91.6521365566204,
4.60515113326408));
#13680=CARTESIAN_POINT('Ctrl Pts',(-208.57976795423,-94.3748341177099,4.76405945206838));
#13681=CARTESIAN_POINT('Ctrl Pts',(-207.464357231459,-97.6706767723307,
4.92296777087269));
#13682=CARTESIAN_POINT('Ctrl Pts',(-204.089651342497,-98.5180728116819,
5.081876089677));
#13683=CARTESIAN_POINT('Ctrl Pts',(-202.125612631896,-96.6794292344261,
5.20474568366028));
#13684=CARTESIAN_POINT('Ctrl Pts',(-201.926398319301,-95.3300541428894,
5.27464583804213));
#13685=CARTESIAN_POINT('Ctrl Pts',(-201.928899855331,-95.0025004707799,
5.29157655282255));
#13686=CARTESIAN_POINT('Ctrl Pts',(-201.931412543801,-95.0002813817275,
4.20842344717746));
#13687=CARTESIAN_POINT('Ctrl Pts',(-201.931845200035,-94.4697309905534,
4.2357905006904));
#13688=CARTESIAN_POINT('Ctrl Pts',(-202.315173521402,-92.9117048313377,
4.31612699380478));
#13689=CARTESIAN_POINT('Ctrl Pts',(-204.794830735755,-91.3718494664313,
4.44943292652058));
#13690=CARTESIAN_POINT('Ctrl Pts',(-207.938821267524,-92.8625013967925,
4.60834124532489));
#13691=CARTESIAN_POINT('Ctrl Pts',(-208.38853330781,-96.3127881561792,4.7672495641292));
#13692=CARTESIAN_POINT('Ctrl Pts',(-205.731675884439,-98.55952540675,4.92615788293351));
#13693=CARTESIAN_POINT('Ctrl Pts',(-202.652180845941,-97.6187407126683,
5.07321584394959));
#13694=CARTESIAN_POINT('Ctrl Pts',(-201.933431315907,-95.790865204812,5.16730436536424));
#13695=CARTESIAN_POINT('Ctrl Pts',(-201.926089504652,-94.997192970312,5.20842344717746));
#13696=CARTESIAN_POINT('Origin',(-205.,-95.,-2.20842344717744));
#13697=CARTESIAN_POINT('',(-201.92505449297,-95.0026812154856,3.20842344717746));
#13698=CARTESIAN_POINT('',(-201.927395781804,-94.9972100788545,3.29157655282255));
#13699=CARTESIAN_POINT('',(-201.9265,-94.9999999999997,-2.20842344717744));
#13700=CARTESIAN_POINT('Ctrl Pts',(-201.927395781804,-94.9972100788545,
3.29157655282255));
#13701=CARTESIAN_POINT('Ctrl Pts',(-201.924984715586,-94.7247076994421,
3.30567922949157));
#13702=CARTESIAN_POINT('Ctrl Pts',(-202.083098692961,-93.431441735486,3.37275134576203));
#13703=CARTESIAN_POINT('Ctrl Pts',(-203.9034944657,-91.5354298104801,3.49279290163393));
#13704=CARTESIAN_POINT('Ctrl Pts',(-207.318557571481,-92.2018109830213,
3.65170122043824));
#13705=CARTESIAN_POINT('Ctrl Pts',(-208.607993009848,-95.4335405719414,
3.81060953924254));
#13706=CARTESIAN_POINT('Ctrl Pts',(-206.589660782539,-98.2678050099089,
3.96951785804685));
#13707=CARTESIAN_POINT('Ctrl Pts',(-203.113945317127,-98.1061823384649,
4.12842617685115));
#13708=CARTESIAN_POINT('Ctrl Pts',(-201.934002400455,-96.0731803187063,
4.23577907510972));
#13709=CARTESIAN_POINT('Ctrl Pts',(-201.921353503737,-95.0276917130945,
4.29016253376686));
#13710=CARTESIAN_POINT('Ctrl Pts',(-201.921415568031,-95.0005065249549,
4.29157655282255));
#13711=CARTESIAN_POINT('Ctrl Pts',(-201.92505449297,-95.0026812154857,3.20842344717746));
#13712=CARTESIAN_POINT('Ctrl Pts',(-201.932628937064,-94.1756633460531,
3.25130719641512));
#13713=CARTESIAN_POINT('Ctrl Pts',(-202.703262857742,-92.3146803557045,
3.34716038525422));
#13714=CARTESIAN_POINT('Ctrl Pts',(-205.849650506345,-91.4667770036684,
3.49598301369474));
#13715=CARTESIAN_POINT('Ctrl Pts',(-208.430318355407,-93.8006307060494,
3.65489133249905));
#13716=CARTESIAN_POINT('Ctrl Pts',(-207.866108674953,-97.2340527708336,
3.81379965130336));
#13717=CARTESIAN_POINT('Ctrl Pts',(-204.674282595805,-98.6193202254382,
3.97270797010767));
#13718=CARTESIAN_POINT('Ctrl Pts',(-202.279337066252,-97.0193151145692,
4.10424923539903));
#13719=CARTESIAN_POINT('Ctrl Pts',(-201.931007785871,-95.4966211118274,
4.18282106108896));
#13720=CARTESIAN_POINT('Ctrl Pts',(-201.931412543801,-95.0002813817275,
4.20842344717746));
#13721=CARTESIAN_POINT('Origin',(-205.,-95.,-2.20842344717744));
#13722=CARTESIAN_POINT('',(-201.922621816358,-94.9982129686146,2.20842344717746));
#13723=CARTESIAN_POINT('',(-201.931144087497,-95.0009810700816,2.29157655282255));
#13724=CARTESIAN_POINT('',(-201.9265,-94.9999999999997,-2.20842344717744));
#13725=CARTESIAN_POINT('Ctrl Pts',(-201.931144087497,-95.0009810700815,
2.29157655282255));
#13726=CARTESIAN_POINT('Ctrl Pts',(-201.93278473837,-94.4268914775859,2.32119592521629));
#13727=CARTESIAN_POINT('Ctrl Pts',(-202.363262699554,-92.8238514576806,
2.40378473721147));
#13728=CARTESIAN_POINT('Ctrl Pts',(-204.94900324081,-91.3664108391532,2.53934298880809));
#13729=CARTESIAN_POINT('Ctrl Pts',(-208.026893856913,-92.9891582387231,
2.6982513076124));
#13730=CARTESIAN_POINT('Ctrl Pts',(-208.329762022302,-96.4554229209582,
2.8571596264167));
#13731=CARTESIAN_POINT('Ctrl Pts',(-205.579941578641,-98.5873721213763,
3.01606794522101));
#13732=CARTESIAN_POINT('Ctrl Pts',(-202.589661678081,-97.5331315540107,
3.16087358735629));
#13733=CARTESIAN_POINT('Ctrl Pts',(-201.934040643722,-95.748222502078,3.25270978989014));
#13734=CARTESIAN_POINT('Ctrl Pts',(-201.927395781804,-94.9972100788545,
3.29157655282255));
#13735=CARTESIAN_POINT('Ctrl Pts',(-201.922621816358,-94.9982129686145,
2.20842344717746));
#13736=CARTESIAN_POINT('Ctrl Pts',(-201.921899400381,-94.8936907064347,
2.2138544525384));
#13737=CARTESIAN_POINT('Ctrl Pts',(-201.974189338711,-93.7704778816497,
2.27225489750078));
#13738=CARTESIAN_POINT('Ctrl Pts',(-203.3543200081,-91.7600452157265,2.3836247820646));
#13739=CARTESIAN_POINT('Ctrl Pts',(-206.83230253,-91.8618097110707,2.5425331008689));
#13740=CARTESIAN_POINT('Ctrl Pts',(-208.630450771479,-94.8406321802388,
2.70144141967321));
#13741=CARTESIAN_POINT('Ctrl Pts',(-207.100242225817,-97.9655611925551,
2.86034973847752));
#13742=CARTESIAN_POINT('Ctrl Pts',(-203.644555128245,-98.3716968938806,
3.01925805728183));
#13743=CARTESIAN_POINT('Ctrl Pts',(-202.028743553123,-96.4112848780084,
3.13528262684847));
#13744=CARTESIAN_POINT('Ctrl Pts',(-201.923273083948,-95.1971848749064,
3.19833775681368));
#13745=CARTESIAN_POINT('Ctrl Pts',(-201.92505449297,-95.0026812154857,3.20842344717746));
#13746=CARTESIAN_POINT('Origin',(-205.,-95.,-2.20842344717744));
#13747=CARTESIAN_POINT('',(-201.930545885435,-94.9983467356882,1.20842344717746));
#13748=CARTESIAN_POINT('',(-201.923792845874,-95.0023469955484,1.29157655282255));
#13749=CARTESIAN_POINT('',(-201.9265,-94.9999999999997,-2.20842344717744));
#13750=CARTESIAN_POINT('Ctrl Pts',(-201.923792845874,-95.0023469955484,
1.29157655282255));
#13751=CARTESIAN_POINT('Ctrl Pts',(-201.931146827165,-94.1328175962329,
1.33671262094101));
#13752=CARTESIAN_POINT('Ctrl Pts',(-202.771183473608,-92.2304180348085,
1.43481812866091));
#13753=CARTESIAN_POINT('Ctrl Pts',(-205.99884385808,-91.5060233304403,1.58589307598225));
#13754=CARTESIAN_POINT('Ctrl Pts',(-208.478131419088,-93.947301914462,1.74480139478656));
#13755=CARTESIAN_POINT('Ctrl Pts',(-207.768707464389,-97.3536847345279,
1.90370971359086));
#13756=CARTESIAN_POINT('Ctrl Pts',(-204.520963212211,-98.6022345372543,
2.06261803239517));
#13757=CARTESIAN_POINT('Ctrl Pts',(-202.235891711733,-96.9311358694141,
2.19190697880573));
#13758=CARTESIAN_POINT('Ctrl Pts',(-201.929850700601,-95.4535575254436,
2.26822648561486));
#13759=CARTESIAN_POINT('Ctrl Pts',(-201.931144087497,-95.0009810700815,
2.29157655282255));
#13760=CARTESIAN_POINT('Ctrl Pts',(-201.930545885435,-94.9983467356882,
1.20842344717746));
#13761=CARTESIAN_POINT('Ctrl Pts',(-201.928558487872,-94.5925295358999,
1.22937114826312));
#13762=CARTESIAN_POINT('Ctrl Pts',(-202.192304255167,-93.1630157504797,
1.30328828895022));
#13763=CARTESIAN_POINT('Ctrl Pts',(-204.358397024947,-91.4231516694834,
1.43017486923876));
#13764=CARTESIAN_POINT('Ctrl Pts',(-207.659318082557,-92.523390293429,1.58908318804306));
#13765=CARTESIAN_POINT('Ctrl Pts',(-208.522221650421,-95.8941719984357,
1.74799150684737));
#13766=CARTESIAN_POINT('Ctrl Pts',(-206.155984228169,-98.445179562461,1.90689982565168));
#13767=CARTESIAN_POINT('Ctrl Pts',(-202.847048276294,-97.8584507200909,
2.06037713909504));
#13768=CARTESIAN_POINT('Ctrl Pts',(-201.92894523571,-95.9131125787372,2.16088501293697));
#13769=CARTESIAN_POINT('Ctrl Pts',(-201.922621816358,-94.9982129686145,
2.20842344717746));
#13770=CARTESIAN_POINT('Origin',(-205.,-95.,-2.20842344717744));
#13771=CARTESIAN_POINT('',(-201.929615858992,-95.0031001153078,0.208423447177458));
#13772=CARTESIAN_POINT('',(-201.92372071423,-94.9977231567353,0.291576552822548));
#13773=CARTESIAN_POINT('',(-201.9265,-94.9999999999997,-2.20842344717744));
#13774=CARTESIAN_POINT('',(-204.206200717467,-97.9692229537457,0.));
#13775=CARTESIAN_POINT('Ctrl Pts',(-204.206200717467,-97.9692229537457,
-1.94289029309402E-15));
#13776=CARTESIAN_POINT('Ctrl Pts',(-203.217993421758,-97.7050332130129,
0.0529694396014337));
#13777=CARTESIAN_POINT('Ctrl Pts',(-202.119889495333,-96.6624088612686,
0.12244392199392));
#13778=CARTESIAN_POINT('Ctrl Pts',(-201.927197987239,-95.3223298493217,
0.191918404386407));
#13779=CARTESIAN_POINT('Ctrl Pts',(-201.929615858992,-95.0031001153078,
0.208423447177458));
#13780=CARTESIAN_POINT('',(-205.795569492778,-97.9745894933442,-2.18341408843227E-15));
#13781=CARTESIAN_POINT('Origin',(-205.,-95.,0.));
#13782=CARTESIAN_POINT('Ctrl Pts',(-205.795570948431,-97.9745939062759,
-4.32461141550156E-16));
#13783=CARTESIAN_POINT('Ctrl Pts',(-204.831203870468,-98.23107300128,0.0519060689144959));
#13784=CARTESIAN_POINT('Ctrl Pts',(-202.766510494357,-97.7537503538027,
0.149098253188679));
#13785=CARTESIAN_POINT('Ctrl Pts',(-201.931000984951,-95.8699154848355,
0.246290437462861));
#13786=CARTESIAN_POINT('Ctrl Pts',(-201.92372071423,-94.9977231567353,0.291576552822548));
#13787=CARTESIAN_POINT('Origin',(-205.,65.,9.));
#13788=CARTESIAN_POINT('',(-202.486496179335,65.0006394388502,16.6125833024919));
#13789=CARTESIAN_POINT('',(-202.48457052599,64.9962980322032,16.8874166975081));
#13790=CARTESIAN_POINT('',(-202.4825,65.,9.));
#13791=CARTESIAN_POINT('',(-203.086534003335,66.6359872033749,17.));
#13792=CARTESIAN_POINT('Ctrl Pts',(-202.48457052599,64.9962980322032,16.8874166975081));
#13793=CARTESIAN_POINT('Ctrl Pts',(-202.489762931999,65.5889737230783,16.9249444650054));
#13794=CARTESIAN_POINT('Ctrl Pts',(-202.700778171916,66.1848035603044,16.9624722325027));
#13795=CARTESIAN_POINT('Ctrl Pts',(-203.086534003335,66.6359872033749,17.));
#13796=CARTESIAN_POINT('',(-202.4825,65.,17.));
#13797=CARTESIAN_POINT('Origin',(-205.,65.,17.));
#13798=CARTESIAN_POINT('',(-202.4825,65.,18.));
#13799=CARTESIAN_POINT('',(-202.4825,65.,9.));
#13800=CARTESIAN_POINT('Origin',(-205.,65.,18.));
#13801=CARTESIAN_POINT('',(-206.917145133663,66.6387833132748,17.));
#13802=CARTESIAN_POINT('Origin',(-205.,65.,17.));
#13803=CARTESIAN_POINT('Ctrl Pts',(-206.917148172614,66.6387856228499,17.));
#13804=CARTESIAN_POINT('Ctrl Pts',(-206.385177397257,67.2593634683583,16.9480939310855));
#13805=CARTESIAN_POINT('Ctrl Pts',(-205.522587697278,67.5988758107765,16.896187862171));
#13806=CARTESIAN_POINT('Ctrl Pts',(-204.71052147175,67.5049508117595,16.8442817932565));
#13807=CARTESIAN_POINT('Ctrl Pts',(-203.881818898331,67.4091016236675,16.791312353655));
#13808=CARTESIAN_POINT('Ctrl Pts',(-203.105731096268,66.8618740047602,16.7383429140536));
#13809=CARTESIAN_POINT('Ctrl Pts',(-202.737501947155,66.1136053435159,16.6853734744522));
#13810=CARTESIAN_POINT('Ctrl Pts',(-202.568829449161,65.7708504460112,16.6611100837988));
#13811=CARTESIAN_POINT('Ctrl Pts',(-202.485734906376,65.3859125981344,16.6368466931454));
#13812=CARTESIAN_POINT('Ctrl Pts',(-202.486496179335,65.0006394388502,16.6125833024919));
#13813=CARTESIAN_POINT('Origin',(-205.,65.,9.));
#13814=CARTESIAN_POINT('',(-202.482814461221,64.9976897634636,15.6125833024919));
#13815=CARTESIAN_POINT('',(-202.478263011551,65.0000328308196,15.8874166975081));
#13816=CARTESIAN_POINT('',(-202.4825,65.,9.));
#13817=CARTESIAN_POINT('Ctrl Pts',(-202.478263011551,65.0000328308196,15.8874166975081));
#13818=CARTESIAN_POINT('Ctrl Pts',(-202.478152266341,65.8352649464484,15.9404611607301));
#13819=CARTESIAN_POINT('Ctrl Pts',(-202.934430616534,66.6703612939895,15.9935056239522));
#13820=CARTESIAN_POINT('Ctrl Pts',(-203.637206972926,67.1217640108908,16.0465500871742));
#13821=CARTESIAN_POINT('Ctrl Pts',(-204.33898935514,67.5725282847932,16.0995195267756));
#13822=CARTESIAN_POINT('Ctrl Pts',(-205.286572131988,67.6406835188332,16.1524889663771));
#13823=CARTESIAN_POINT('Ctrl Pts',(-206.045557105916,67.2948210424227,16.2054584059785));
#13824=CARTESIAN_POINT('Ctrl Pts',(-206.804542079844,66.9489585660121,16.2584278455799));
#13825=CARTESIAN_POINT('Ctrl Pts',(-207.374929250853,66.1890783791509,16.3113972851814));
#13826=CARTESIAN_POINT('Ctrl Pts',(-207.495321313456,65.3638484600988,16.3643667247828));
#13827=CARTESIAN_POINT('Ctrl Pts',(-207.61571337606,64.5386185410466,16.4173361643842));
#13828=CARTESIAN_POINT('Ctrl Pts',(-207.286110330258,63.6480388898036,16.4703056039857));
#13829=CARTESIAN_POINT('Ctrl Pts',(-206.657467900973,63.0996378515271,16.5232750435871));
#13830=CARTESIAN_POINT('Ctrl Pts',(-206.028825471689,62.5512368132507,16.5762444831886));
#13831=CARTESIAN_POINT('Ctrl Pts',(-205.101143658922,62.3450143879409,16.62921392279));
#13832=CARTESIAN_POINT('Ctrl Pts',(-204.29994880059,62.5769614457771,16.6821833623914));
#13833=CARTESIAN_POINT('Ctrl Pts',(-203.498753942257,62.8089085036132,16.7351528019929));
#13834=CARTESIAN_POINT('Ctrl Pts',(-202.824046038359,63.4790250445952,16.7881222415943));
#13835=CARTESIAN_POINT('Ctrl Pts',(-202.584870045267,64.2765863098395,16.8410916811957));
#13836=CARTESIAN_POINT('Ctrl Pts',(-202.515145364615,64.5090916871573,16.8565333532998));
#13837=CARTESIAN_POINT('Ctrl Pts',(-202.482433989863,64.7524278450617,16.871975025404));
#13838=CARTESIAN_POINT('Ctrl Pts',(-202.48457052599,64.9962980322032,16.8874166975081));
#13839=CARTESIAN_POINT('Ctrl Pts',(-202.486496179335,65.0006394388502,16.6125833024919));
#13840=CARTESIAN_POINT('Ctrl Pts',(-202.48739684236,64.5448222644593,16.5838772535439));
#13841=CARTESIAN_POINT('Ctrl Pts',(-202.60567289555,64.0885357450751,16.5551712045959));
#13842=CARTESIAN_POINT('Ctrl Pts',(-202.838472440105,63.7010804418779,16.5264651556478));
#13843=CARTESIAN_POINT('Ctrl Pts',(-203.268042578331,62.9861339050655,16.4734957160464));
#13844=CARTESIAN_POINT('Ctrl Pts',(-204.087553350947,62.5055505350222,16.420526276445));
#13845=CARTESIAN_POINT('Ctrl Pts',(-204.92122518277,62.4795075785488,16.3675568368436));
#13846=CARTESIAN_POINT('Ctrl Pts',(-205.754897014594,62.4534646220754,16.3145873972421));
#13847=CARTESIAN_POINT('Ctrl Pts',(-206.602729905625,62.8819620791719,16.2616179576407));
#13848=CARTESIAN_POINT('Ctrl Pts',(-207.07614049038,63.5686371465989,16.2086485180392));
#13849=CARTESIAN_POINT('Ctrl Pts',(-207.549551075135,64.255312214026,16.1556790784378));
#13850=CARTESIAN_POINT('Ctrl Pts',(-207.648539353615,65.2001648917836,16.1027096388364));
#13851=CARTESIAN_POINT('Ctrl Pts',(-207.32770123824,65.9700518006814,16.0497401992349));
#13852=CARTESIAN_POINT('Ctrl Pts',(-207.006863122865,66.7399387095791,15.9967707596335));
#13853=CARTESIAN_POINT('Ctrl Pts',(-206.266198613636,67.334859849617,15.9438013200321));
#13854=CARTESIAN_POINT('Ctrl Pts',(-205.445237984819,67.4821203893694,15.8908318804306));
#13855=CARTESIAN_POINT('Ctrl Pts',(-204.624277356003,67.6293809291217,15.8378624408292));
#13856=CARTESIAN_POINT('Ctrl Pts',(-203.7230206076,67.3289808685885,15.7848930012278));
#13857=CARTESIAN_POINT('Ctrl Pts',(-203.15459209185,66.7186152645058,15.7319235616263));
#13858=CARTESIAN_POINT('Ctrl Pts',(-202.727701876918,66.2602302667535,15.6921434752482));
#13859=CARTESIAN_POINT('Ctrl Pts',(-202.488527469465,65.6270240651797,15.6523633888701));
#13860=CARTESIAN_POINT('Ctrl Pts',(-202.482814461221,64.9976897634636,15.6125833024919));
#13861=CARTESIAN_POINT('Origin',(-205.,65.,9.));
#13862=CARTESIAN_POINT('',(-202.478480714095,65.0006753766358,14.6125833024919));
#13863=CARTESIAN_POINT('',(-202.48391344512,65.0021895194833,14.8874166975081));
#13864=CARTESIAN_POINT('',(-202.4825,65.,9.));
#13865=CARTESIAN_POINT('Ctrl Pts',(-202.48391344512,65.0021895194833,14.8874166975081));
#13866=CARTESIAN_POINT('Ctrl Pts',(-202.481864131876,65.2491292700526,14.9030084168534));
#13867=CARTESIAN_POINT('Ctrl Pts',(-202.515267256566,65.4955265999556,14.9186001361987));
#13868=CARTESIAN_POINT('Ctrl Pts',(-202.58638727583,65.7305084281609,14.9341918555441));
#13869=CARTESIAN_POINT('Ctrl Pts',(-202.828001909944,66.5288075432794,14.9871612951455));
#13870=CARTESIAN_POINT('Ctrl Pts',(-203.504926567004,67.1953544989996,15.0401307347469));
#13871=CARTESIAN_POINT('Ctrl Pts',(-204.306862968527,67.4246089596421,15.0931001743484));
#13872=CARTESIAN_POINT('Ctrl Pts',(-205.10879937005,67.6538634202845,15.1460696139498));
#13873=CARTESIAN_POINT('Ctrl Pts',(-206.035747516037,67.4458253858491,15.1990390535512));
#13874=CARTESIAN_POINT('Ctrl Pts',(-206.662799141937,66.8958561385943,15.2520084931527));
#13875=CARTESIAN_POINT('Ctrl Pts',(-207.289850767837,66.3458868913395,15.3049779327541));
#13876=CARTESIAN_POINT('Ctrl Pts',(-207.617005873651,65.4539864312653,15.3579473723555));
#13877=CARTESIAN_POINT('Ctrl Pts',(-207.494299240605,64.6290014535642,15.410916811957));
#13878=CARTESIAN_POINT('Ctrl Pts',(-207.37159260756,63.8040164758631,15.4638862515584));
#13879=CARTESIAN_POINT('Ctrl Pts',(-206.799024235656,63.0459469805351,15.5168556911598));
#13880=CARTESIAN_POINT('Ctrl Pts',(-206.039054509905,62.7022785064846,15.5698251307613));
#13881=CARTESIAN_POINT('Ctrl Pts',(-205.279084784155,62.358610032434,15.6227945703627));
#13882=CARTESIAN_POINT('Ctrl Pts',(-204.331713704558,62.4293425796608,15.6757640099641));
#13883=CARTESIAN_POINT('Ctrl Pts',(-203.631214496525,62.8820718503695,15.7287334495656));
#13884=CARTESIAN_POINT('Ctrl Pts',(-202.931707445237,63.3341598949429,15.7816278655464));
#13885=CARTESIAN_POINT('Ctrl Pts',(-202.478373443496,64.1671633420724,15.8345222815272));
#13886=CARTESIAN_POINT('Ctrl Pts',(-202.478263011551,65.0000328308196,15.8874166975081));
#13887=CARTESIAN_POINT('Ctrl Pts',(-202.482814461221,64.9976897634636,15.6125833024919));
#13888=CARTESIAN_POINT('Ctrl Pts',(-202.480920275196,64.7890297740916,15.5993939492686));
#13889=CARTESIAN_POINT('Ctrl Pts',(-202.504690461007,64.5807954220112,15.5862045960453));
#13890=CARTESIAN_POINT('Ctrl Pts',(-202.555792352561,64.3794997079143,15.573015242822));
#13891=CARTESIAN_POINT('Ctrl Pts',(-202.761021412117,63.5710809030377,15.5200458032206));
#13892=CARTESIAN_POINT('Ctrl Pts',(-203.407079814325,62.8745744409167,15.4670763636191));
#13893=CARTESIAN_POINT('Ctrl Pts',(-204.197816415991,62.6092534217428,15.4141069240177));
#13894=CARTESIAN_POINT('Ctrl Pts',(-204.988553017657,62.343932402569,15.3611374844163));
#13895=CARTESIAN_POINT('Ctrl Pts',(-205.92396781878,62.5097968263422,15.3081680448148));
#13896=CARTESIAN_POINT('Ctrl Pts',(-206.575272670495,63.0308161306152,15.2551986052134));
#13897=CARTESIAN_POINT('Ctrl Pts',(-207.226577522209,63.5518354348882,15.202229165612));
#13898=CARTESIAN_POINT('Ctrl Pts',(-207.593772424515,64.4280096196609,15.1492597260105));
#13899=CARTESIAN_POINT('Ctrl Pts',(-207.508536912918,65.2577049646526,15.0962902864091));
#13900=CARTESIAN_POINT('Ctrl Pts',(-207.423301401321,66.0874003096444,15.0433208468077));
#13901=CARTESIAN_POINT('Ctrl Pts',(-206.885635475823,66.8706168148552,14.9903514072062));
#13902=CARTESIAN_POINT('Ctrl Pts',(-206.142002373318,67.2483325911416,14.9373819676048));
#13903=CARTESIAN_POINT('Ctrl Pts',(-205.398369270814,67.6260483674281,14.8844125280034));
#13904=CARTESIAN_POINT('Ctrl Pts',(-204.448768991303,67.5982634147903,14.8314430884019));
#13905=CARTESIAN_POINT('Ctrl Pts',(-203.728492908084,67.1777141128455,14.7784736488005));
#13906=CARTESIAN_POINT('Ctrl Pts',(-203.008216824865,66.7571648109008,14.725504209199));
#13907=CARTESIAN_POINT('Ctrl Pts',(-202.517264937938,65.9438511596491,14.6725347695976));
#13908=CARTESIAN_POINT('Ctrl Pts',(-202.480686891426,65.1105916341598,14.6195653299962));
#13909=CARTESIAN_POINT('Ctrl Pts',(-202.479079745062,65.0739803291702,14.6172379874948));
#13910=CARTESIAN_POINT('Ctrl Pts',(-202.478349767474,65.0373305186669,14.6149106449934));
#13911=CARTESIAN_POINT('Ctrl Pts',(-202.478480714095,65.0006753766358,14.6125833024919));
#13912=CARTESIAN_POINT('Origin',(-205.,65.,9.));
#13913=CARTESIAN_POINT('',(-202.484829356871,65.0019240714538,13.6125833024919));
#13914=CARTESIAN_POINT('',(-202.48603693456,64.9988431445427,13.8874166975081));
#13915=CARTESIAN_POINT('',(-202.4825,65.,9.));
#13916=CARTESIAN_POINT('Ctrl Pts',(-202.48603693456,64.9988431445427,13.8874166975081));
#13917=CARTESIAN_POINT('Ctrl Pts',(-202.488081702897,65.4925818678139,13.9185251125781));
#13918=CARTESIAN_POINT('Ctrl Pts',(-202.628468449655,65.9873937525298,13.9496335276482));
#13919=CARTESIAN_POINT('Ctrl Pts',(-202.899518895525,66.3954024519509,13.9807419427182));
#13920=CARTESIAN_POINT('Ctrl Pts',(-203.361046433623,67.0901338329029,14.0337113823196));
#13921=CARTESIAN_POINT('Ctrl Pts',(-204.201408831768,67.5331956776596,14.0866808219211));
#13922=CARTESIAN_POINT('Ctrl Pts',(-205.035388665575,67.5214909265688,14.1396502615225));
#13923=CARTESIAN_POINT('Ctrl Pts',(-205.869368499381,67.509786175478,14.192619701124));
#13924=CARTESIAN_POINT('Ctrl Pts',(-206.69696576885,67.0433148285397,14.2455891407254));
#13925=CARTESIAN_POINT('Ctrl Pts',(-207.13881450515,66.3359047155866,14.2985585803268));
#13926=CARTESIAN_POINT('Ctrl Pts',(-207.580663241451,65.6284946026335,14.3515280199283));
#13927=CARTESIAN_POINT('Ctrl Pts',(-207.636763444583,64.6801457236657,14.4044974595297));
#13928=CARTESIAN_POINT('Ctrl Pts',(-207.281399106155,63.9255759642922,14.4574668991311));
#13929=CARTESIAN_POINT('Ctrl Pts',(-206.926034767727,63.1710062049186,14.5104363387326));
#13930=CARTESIAN_POINT('Ctrl Pts',(-206.159205887739,62.6102155651394,14.563405778334));
#13931=CARTESIAN_POINT('Ctrl Pts',(-205.332422516349,62.5002672183578,14.6163752179354));
#13932=CARTESIAN_POINT('Ctrl Pts',(-204.505639144959,62.3903188715762,14.6693446575369));
#13933=CARTESIAN_POINT('Ctrl Pts',(-203.618901282167,62.7312128177923,14.7223140971383));
#13934=CARTESIAN_POINT('Ctrl Pts',(-203.078684656356,63.3666854281588,14.7752835367397));
#13935=CARTESIAN_POINT('Ctrl Pts',(-202.697482475075,63.8151046985801,14.8126612569959));
#13936=CARTESIAN_POINT('Ctrl Pts',(-202.488826223208,64.4102057419109,14.850038977252));
#13937=CARTESIAN_POINT('Ctrl Pts',(-202.48391344512,65.0021895194833,14.8874166975081));
#13938=CARTESIAN_POINT('Ctrl Pts',(-202.478480714095,65.0006753766358,14.6125833024919));
#13939=CARTESIAN_POINT('Ctrl Pts',(-202.481330063292,64.2030732786072,14.5619412053919));
#13940=CARTESIAN_POINT('Ctrl Pts',(-202.891810860674,63.4029468022227,14.5112991082919));
#13941=CARTESIAN_POINT('Ctrl Pts',(-203.54255899523,62.9420800015405,14.4606570111919));
#13942=CARTESIAN_POINT('Ctrl Pts',(-204.223213351645,62.4600332941377,14.4076875715904));
#13943=CARTESIAN_POINT('Ctrl Pts',(-205.166726270573,62.349145279059,14.354718131989));
#13944=CARTESIAN_POINT('Ctrl Pts',(-205.940596712799,62.6602464127481,14.3017486923876));
#13945=CARTESIAN_POINT('Ctrl Pts',(-206.714467155025,62.9713475464372,14.2487792527861));
#13946=CARTESIAN_POINT('Ctrl Pts',(-207.318695120548,63.7044378288941,14.1958098131847));
#13947=CARTESIAN_POINT('Ctrl Pts',(-207.476305881734,64.5234727665736,14.1428403735833));
#13948=CARTESIAN_POINT('Ctrl Pts',(-207.63391664292,65.3425077042531,14.0898709339818));
#13949=CARTESIAN_POINT('Ctrl Pts',(-207.344910199768,66.2474872971551,14.0369014943804));
#13950=CARTESIAN_POINT('Ctrl Pts',(-206.74176549312,66.8235739596422,13.9839320547789));
#13951=CARTESIAN_POINT('Ctrl Pts',(-206.138620786471,67.3996606221293,13.9309626151775));
#13952=CARTESIAN_POINT('Ctrl Pts',(-205.221337816326,67.6468543542013,13.8779931755761));
#13953=CARTESIAN_POINT('Ctrl Pts',(-204.4103939689,67.4518429293449,13.8250237359746));
#13954=CARTESIAN_POINT('Ctrl Pts',(-203.599450121474,67.2568315044885,13.7720542963732));
#13955=CARTESIAN_POINT('Ctrl Pts',(-202.894845396768,66.6196149227036,13.7190848567718));
#13956=CARTESIAN_POINT('Ctrl Pts',(-202.619566663537,65.8322897046192,13.6661154171703));
#13957=CARTESIAN_POINT('Ctrl Pts',(-202.526832357198,65.5670601421846,13.6482713789442));
#13958=CARTESIAN_POINT('Ctrl Pts',(-202.482819782445,65.2847956160355,13.6304273407181));
#13959=CARTESIAN_POINT('Ctrl Pts',(-202.484829356871,65.0019240714538,13.6125833024919));
#13960=CARTESIAN_POINT('Origin',(-205.,65.,9.));
#13961=CARTESIAN_POINT('',(-202.485436378814,64.9983728001324,12.6125833024919));
#13962=CARTESIAN_POINT('',(-202.479673360095,64.9983441228843,12.8874166975081));
#13963=CARTESIAN_POINT('',(-202.4825,65.,9.));
#13964=CARTESIAN_POINT('Ctrl Pts',(-202.479673360095,64.9983441228843,12.8874166975081));
#13965=CARTESIAN_POINT('Ctrl Pts',(-202.48526219209,65.7335978500889,12.9340418083028));
#13966=CARTESIAN_POINT('Ctrl Pts',(-202.82574540688,66.473357371898,12.9806669190976));
#13967=CARTESIAN_POINT('Ctrl Pts',(-203.391061399314,66.9417737892996,13.0272920298924));
#13968=CARTESIAN_POINT('Ctrl Pts',(-204.033300544841,67.4739281307464,13.0802614694938));
#13969=CARTESIAN_POINT('Ctrl Pts',(-204.965721796711,67.655871464688,13.1332309090952));
#13970=CARTESIAN_POINT('Ctrl Pts',(-205.760908463841,67.4042019838009,13.1862003486967));
#13971=CARTESIAN_POINT('Ctrl Pts',(-206.556095130971,67.1525325029139,13.2391697882981));
#13972=CARTESIAN_POINT('Ctrl Pts',(-207.214047213361,66.467250207198,13.2921392278995));
#13973=CARTESIAN_POINT('Ctrl Pts',(-207.433163153269,65.6624846710021,13.345108667501));
#13974=CARTESIAN_POINT('Ctrl Pts',(-207.652279093177,64.8577191348062,13.3980781071024));
#13975=CARTESIAN_POINT('Ctrl Pts',(-207.432558890604,63.9334703581302,13.4510475467039));
#13976=CARTESIAN_POINT('Ctrl Pts',(-206.874721058672,63.3134088159122,13.5040169863053));
#13977=CARTESIAN_POINT('Ctrl Pts',(-206.31688322674,62.6933472736942,13.5569864259067));
#13978=CARTESIAN_POINT('Ctrl Pts',(-205.420927765449,62.377472965934,13.6099558655082));
#13979=CARTESIAN_POINT('Ctrl Pts',(-204.597555650998,62.5105809084757,13.6629253051096));
#13980=CARTESIAN_POINT('Ctrl Pts',(-203.774183536547,62.6436888510174,13.715894744711));
#13981=CARTESIAN_POINT('Ctrl Pts',(-203.023394768935,63.2257790438609,13.7688641843125));
#13982=CARTESIAN_POINT('Ctrl Pts',(-202.689346724155,63.9900245988563,13.8218336239139));
#13983=CARTESIAN_POINT('Ctrl Pts',(-202.551481710733,64.305436484492,13.8436946484453));
#13984=CARTESIAN_POINT('Ctrl Pts',(-202.484600000834,64.6518748301101,13.8655556729767));
#13985=CARTESIAN_POINT('Ctrl Pts',(-202.48603693456,64.9988431445427,13.8874166975081));
#13986=CARTESIAN_POINT('Ctrl Pts',(-202.484829356871,65.0019240714538,13.6125833024919));
#13987=CARTESIAN_POINT('Ctrl Pts',(-202.488785137923,64.4451007551634,13.5774579011166));
#13988=CARTESIAN_POINT('Ctrl Pts',(-202.671070421135,63.8859253258832,13.5423324997413));
#13989=CARTESIAN_POINT('Ctrl Pts',(-203.0110940357,63.4497025812941,13.507207098366));
#13990=CARTESIAN_POINT('Ctrl Pts',(-203.523852882846,62.7918745304371,13.4542376587646));
#13991=CARTESIAN_POINT('Ctrl Pts',(-204.395323318893,62.4136522831071,13.4012682191632));
#13992=CARTESIAN_POINT('Ctrl Pts',(-205.226028166212,62.4884108039558,13.3482987795617));
#13993=CARTESIAN_POINT('Ctrl Pts',(-206.05673301353,62.5631693248045,13.2953293399603));
#13994=CARTESIAN_POINT('Ctrl Pts',(-206.84667227212,63.0909086138319,13.2423599003589));
#13995=CARTESIAN_POINT('Ctrl Pts',(-207.233742200274,63.8297159301003,13.1893904607574));
#13996=CARTESIAN_POINT('Ctrl Pts',(-207.620812128428,64.5685232463688,13.136421021156));
#13997=CARTESIAN_POINT('Ctrl Pts',(-207.605012726144,65.5183985898783,13.0834515815545));
#13998=CARTESIAN_POINT('Ctrl Pts',(-207.193586351169,66.2439244114753,13.0304821419531));
#13999=CARTESIAN_POINT('Ctrl Pts',(-206.782159976194,66.9694502330724,12.9775127023517));
#14000=CARTESIAN_POINT('Ctrl Pts',(-205.975106628526,67.4706265327569,12.9245432627502));
#14001=CARTESIAN_POINT('Ctrl Pts',(-205.142375052588,67.5177168955105,12.8715738231488));
#14002=CARTESIAN_POINT('Ctrl Pts',(-204.30964347665,67.5648072582641,12.8186043835474));
#14003=CARTESIAN_POINT('Ctrl Pts',(-203.451233672441,67.1578116840866,12.7656349439459));
#14004=CARTESIAN_POINT('Ctrl Pts',(-202.960635897084,66.4832946697357,12.7126655043445));
#14005=CARTESIAN_POINT('Ctrl Pts',(-202.651652038019,66.0584764570002,12.6793047703936));
#14006=CARTESIAN_POINT('Ctrl Pts',(-202.48856518007,65.5275426939449,12.6459440364428));
#14007=CARTESIAN_POINT('Ctrl Pts',(-202.485436378814,64.9983728001324,12.6125833024919));
#14008=CARTESIAN_POINT('Origin',(-205.,65.,9.));
#14009=CARTESIAN_POINT('',(-202.478899910386,64.9988537237822,11.6125833024919));
#14010=CARTESIAN_POINT('',(-202.480895712983,65.0021035865431,11.8874166975081));
#14011=CARTESIAN_POINT('',(-202.4825,65.,9.));
#14012=CARTESIAN_POINT('Ctrl Pts',(-202.480895712983,65.0021035865431,11.8874166975081));
#14013=CARTESIAN_POINT('Ctrl Pts',(-202.479598519915,65.1469297626336,11.8965890644261));
#14014=CARTESIAN_POINT('Ctrl Pts',(-202.491010908424,65.2915516069264,11.9057614313442));
#14015=CARTESIAN_POINT('Ctrl Pts',(-202.515857741095,65.4338272778794,11.9149337982622));
#14016=CARTESIAN_POINT('Ctrl Pts',(-202.659345546828,66.2554540865998,11.9679032378637));
#14017=CARTESIAN_POINT('Ctrl Pts',(-203.250863894479,66.998837441384,12.0208726774651));
#14018=CARTESIAN_POINT('Ctrl Pts',(-204.019264079124,67.3232145667187,12.0738421170665));
#14019=CARTESIAN_POINT('Ctrl Pts',(-204.787664263768,67.6475916920535,12.126811556668));
#14020=CARTESIAN_POINT('Ctrl Pts',(-205.732946285406,67.5529625879387,12.1797809962694));
#14021=CARTESIAN_POINT('Ctrl Pts',(-206.421798147929,67.0827047068781,12.2327504358708));
#14022=CARTESIAN_POINT('Ctrl Pts',(-207.110650010453,66.6124468258175,12.2857198754723));
#14023=CARTESIAN_POINT('Ctrl Pts',(-207.543071713862,65.7665601678111,12.3386893150737));
#14024=CARTESIAN_POINT('Ctrl Pts',(-207.520843565857,64.9327944497339,12.3916587546751));
#14025=CARTESIAN_POINT('Ctrl Pts',(-207.498615417853,64.0990287316567,12.4446281942766));
#14026=CARTESIAN_POINT('Ctrl Pts',(-207.021737418434,63.2773839535086,12.497597633878));
#14027=CARTESIAN_POINT('Ctrl Pts',(-206.308807777554,62.8444974899262,12.5505670734795));
#14028=CARTESIAN_POINT('Ctrl Pts',(-205.595878136674,62.4116110263438,12.6035365130809));
#14029=CARTESIAN_POINT('Ctrl Pts',(-204.646896854331,62.367482877327,12.6565059526823));
#14030=CARTESIAN_POINT('Ctrl Pts',(-203.896871647065,62.7323411397584,12.7094753922838));
#14031=CARTESIAN_POINT('Ctrl Pts',(-203.146846439799,63.0971994021897,12.7624448318852));
#14032=CARTESIAN_POINT('Ctrl Pts',(-202.595777307608,63.8710440760693,12.8154142714866));
#14033=CARTESIAN_POINT('Ctrl Pts',(-202.496271261105,64.6991490874851,12.8683837110881));
#14034=CARTESIAN_POINT('Ctrl Pts',(-202.484353085606,64.7983340235237,12.8747280398947));
#14035=CARTESIAN_POINT('Ctrl Pts',(-202.478912881734,64.8982973600521,12.8810723687014));
#14036=CARTESIAN_POINT('Ctrl Pts',(-202.479673360095,64.9983441228843,12.8874166975081));
#14037=CARTESIAN_POINT('Ctrl Pts',(-202.485436378814,64.9983728001324,12.6125833024919));
#14038=CARTESIAN_POINT('Ctrl Pts',(-202.483597338253,64.6873383755837,12.5929745968414));
#14039=CARTESIAN_POINT('Ctrl Pts',(-202.537021084319,64.3769133378432,12.5733658911908));
#14040=CARTESIAN_POINT('Ctrl Pts',(-202.648562957585,64.0890044692285,12.5537571855402));
#14041=CARTESIAN_POINT('Ctrl Pts',(-202.94987353995,63.3112697375966,12.5007877459388));
#14042=CARTESIAN_POINT('Ctrl Pts',(-203.675280451186,62.6978387288571,12.4478183063373));
#14043=CARTESIAN_POINT('Ctrl Pts',(-204.492261217045,62.5299047893222,12.3948488667359));
#14044=CARTESIAN_POINT('Ctrl Pts',(-205.309241982905,62.3619708497873,12.3418794271344));
#14045=CARTESIAN_POINT('Ctrl Pts',(-206.217796603388,62.639533979457,12.288909987533));
#14046=CARTESIAN_POINT('Ctrl Pts',(-206.801448717827,63.2353607908227,12.2359405479316));
#14047=CARTESIAN_POINT('Ctrl Pts',(-207.385100832267,63.8311876021884,12.1829711083301));
#14048=CARTESIAN_POINT('Ctrl Pts',(-207.643850440664,64.7452780952501,12.1300016687287));
#14049=CARTESIAN_POINT('Ctrl Pts',(-207.459088168525,65.5586182962889,12.0770322291273));
#14050=CARTESIAN_POINT('Ctrl Pts',(-207.274325896385,66.3719584973278,12.0240627895258));
#14051=CARTESIAN_POINT('Ctrl Pts',(-206.64605174371,67.0845484063438,11.9710933499244));
#14052=CARTESIAN_POINT('Ctrl Pts',(-205.862263071039,67.3697407912789,11.918123910323));
#14053=CARTESIAN_POINT('Ctrl Pts',(-205.078474398368,67.6549331762139,11.8651544707215));
#14054=CARTESIAN_POINT('Ctrl Pts',(-204.139171205702,67.512728037068,11.8121850311201));
#14055=CARTESIAN_POINT('Ctrl Pts',(-203.47492482736,67.0083114149271,11.7592155915187));
#14056=CARTESIAN_POINT('Ctrl Pts',(-202.861992995554,66.5428621264053,11.7103381618431));
#14057=CARTESIAN_POINT('Ctrl Pts',(-202.483261962138,65.7690030327609,11.6614607321675));
#14058=CARTESIAN_POINT('Ctrl Pts',(-202.478899910386,64.9988537237822,11.6125833024919));
#14059=CARTESIAN_POINT('Origin',(-205.,65.,9.));
#14060=CARTESIAN_POINT('',(-202.481967556149,65.0022835844395,10.6125833024919));
#14061=CARTESIAN_POINT('',(-202.486473208904,65.0004666846809,10.8874166975081));
#14062=CARTESIAN_POINT('',(-202.4825,65.,9.));
#14063=CARTESIAN_POINT('Ctrl Pts',(-202.486473208904,65.0004666846809,10.8874166975081));
#14064=CARTESIAN_POINT('Ctrl Pts',(-202.485824990019,65.3924902192974,10.9121057601508));
#14065=CARTESIAN_POINT('Ctrl Pts',(-202.571984008169,65.784244058827,10.9367948227936));
#14066=CARTESIAN_POINT('Ctrl Pts',(-202.746442526037,66.1316570068074,10.9614838854364));
#14067=CARTESIAN_POINT('Ctrl Pts',(-203.120736603494,66.8770181989703,11.0144533250378));
#14068=CARTESIAN_POINT('Ctrl Pts',(-203.901473819497,67.4182779954878,11.0674227646393));
#14069=CARTESIAN_POINT('Ctrl Pts',(-204.730768597298,67.5073259304104,11.1203922042407));
#14070=CARTESIAN_POINT('Ctrl Pts',(-205.560063375099,67.5963738653331,11.1733616438421));
#14071=CARTESIAN_POINT('Ctrl Pts',(-206.437915714699,67.2332099386611,11.2263310834436));
#14072=CARTESIAN_POINT('Ctrl Pts',(-206.961923009412,66.5843064648767,11.279300523045));
#14073=CARTESIAN_POINT('Ctrl Pts',(-207.485930304125,65.9354029910924,11.3322699626464));
#14074=CARTESIAN_POINT('Ctrl Pts',(-207.656092553952,65.0007599701958,11.3852394022479));
#14075=CARTESIAN_POINT('Ctrl Pts',(-207.394408334505,64.2088125398099,11.4382088418493));
#14076=CARTESIAN_POINT('Ctrl Pts',(-207.132724115059,63.416865109424,11.4911782814507));
#14077=CARTESIAN_POINT('Ctrl Pts',(-206.439193426339,62.7676132695489,11.5441477210522));
#14078=CARTESIAN_POINT('Ctrl Pts',(-205.631726860331,62.5586704353066,11.5971171606536));
#14079=CARTESIAN_POINT('Ctrl Pts',(-204.824260294323,62.3497276010643,11.650086600255));
#14080=CARTESIAN_POINT('Ctrl Pts',(-203.902857851026,62.5810937724549,11.7030560398565));
#14081=CARTESIAN_POINT('Ctrl Pts',(-203.289885261286,63.1467119894785,11.7560254794579));
#14082=CARTESIAN_POINT('Ctrl Pts',(-202.783057073792,63.614385847243,11.7998225521413));
#14083=CARTESIAN_POINT('Ctrl Pts',(-202.48708967138,64.3105740590657,11.8436196248247));
#14084=CARTESIAN_POINT('Ctrl Pts',(-202.480895712983,65.0021035865431,11.8874166975081));
#14085=CARTESIAN_POINT('Ctrl Pts',(-202.478899910386,64.9988537237822,11.6125833024919));
#14086=CARTESIAN_POINT('Ctrl Pts',(-202.478534720171,64.9343769573553,11.6084912925661));
#14087=CARTESIAN_POINT('Ctrl Pts',(-202.48079348564,64.8699261928438,11.6043992826402));
#14088=CARTESIAN_POINT('Ctrl Pts',(-202.485758456508,64.8056845798517,11.6003072727143));
#14089=CARTESIAN_POINT('Ctrl Pts',(-202.550028028015,63.9741024720533,11.5473378331129));
#14090=CARTESIAN_POINT('Ctrl Pts',(-203.067756735046,63.1775663615925,11.4943683935115));
#14091=CARTESIAN_POINT('Ctrl Pts',(-203.801620631571,62.781203950145,11.44139895391));
#14092=CARTESIAN_POINT('Ctrl Pts',(-204.535484528097,62.3848415386974,11.3884295143086));
#14093=CARTESIAN_POINT('Ctrl Pts',(-205.485483614117,62.388652826263,11.3354600747072));
#14094=CARTESIAN_POINT('Ctrl Pts',(-206.216143617571,62.7908907399206,11.2824906351057));
#14095=CARTESIAN_POINT('Ctrl Pts',(-206.946803621026,63.1931286535783,11.2295211955043));
#14096=CARTESIAN_POINT('Ctrl Pts',(-207.458124541916,63.9937931933281,11.1765517559029));
#14097=CARTESIAN_POINT('Ctrl Pts',(-207.515719727568,64.8258642085796,11.1235823163014));
#14098=CARTESIAN_POINT('Ctrl Pts',(-207.57331491322,65.6579352238312,11.0706128767));
#14099=CARTESIAN_POINT('Ctrl Pts',(-207.177184363636,66.5214127145845,11.0176434370986));
#14100=CARTESIAN_POINT('Ctrl Pts',(-206.508912109009,67.0204834245331,10.9646739974971));
#14101=CARTESIAN_POINT('Ctrl Pts',(-205.840639854383,67.5195541344816,10.9117045578957));
#14102=CARTESIAN_POINT('Ctrl Pts',(-204.900225894714,67.6542180636253,10.8587351182942));
#14103=CARTESIAN_POINT('Ctrl Pts',(-204.11875073371,67.3627460194001,10.8057656786928));
#14104=CARTESIAN_POINT('Ctrl Pts',(-203.337275572705,67.0712739751749,10.7527962390914));
#14105=CARTESIAN_POINT('Ctrl Pts',(-202.714739210364,66.3536659575809,10.6998267994899));
#14106=CARTESIAN_POINT('Ctrl Pts',(-202.536508836204,65.5388694716049,10.6468573598885));
#14107=CARTESIAN_POINT('Ctrl Pts',(-202.498067311432,65.3631305188742,10.6354326740897));
#14108=CARTESIAN_POINT('Ctrl Pts',(-202.48029480925,65.1828703787145,10.6240079882908));
#14109=CARTESIAN_POINT('Ctrl Pts',(-202.481967556149,65.0022835844395,10.6125833024919));
#14110=CARTESIAN_POINT('Origin',(-205.,65.,9.));
#14111=CARTESIAN_POINT('',(-202.486546886373,64.9998805727156,9.61258330249194));
#14112=CARTESIAN_POINT('',(-202.482611670102,64.997686958861,9.88741669750806));
#14113=CARTESIAN_POINT('',(-202.4825,65.,9.));
#14114=CARTESIAN_POINT('Ctrl Pts',(-202.482611670102,64.997686958861,9.88741669750806));
#14115=CARTESIAN_POINT('Ctrl Pts',(-202.488432746159,65.6336242075107,9.92762245587555));
#14116=CARTESIAN_POINT('Ctrl Pts',(-202.733277868516,66.2735520171247,9.96782821424304));
#14117=CARTESIAN_POINT('Ctrl Pts',(-203.168440184143,66.7333659482197,10.0080339726105));
#14118=CARTESIAN_POINT('Ctrl Pts',(-203.741748708353,67.3391519659441,10.061003412212));
#14119=CARTESIAN_POINT('Ctrl Pts',(-204.64539046284,67.6323146295356,10.1139728518134));
#14120=CARTESIAN_POINT('Ctrl Pts',(-205.465141117256,67.4784698123131,10.1669422914149));
#14121=CARTESIAN_POINT('Ctrl Pts',(-206.284891771673,67.3246249950906,10.2199117310163));
#14122=CARTESIAN_POINT('Ctrl Pts',(-207.020751326018,66.7237726970541,10.2728811706177));
#14123=CARTESIAN_POINT('Ctrl Pts',(-207.335405872855,65.9513402538225,10.3258506102192));
#14124=CARTESIAN_POINT('Ctrl Pts',(-207.650060419693,65.178907810591,10.3788200498206));
#14125=CARTESIAN_POINT('Ctrl Pts',(-207.543509959022,64.2348952221644,10.431789489422));
#14126=CARTESIAN_POINT('Ctrl Pts',(-207.064596626569,63.5520325835608,10.4847589290235));
#14127=CARTESIAN_POINT('Ctrl Pts',(-206.585683294116,62.8691699449572,10.5377283686249));
#14128=CARTESIAN_POINT('Ctrl Pts',(-205.73440708988,62.4474572561765,10.5906978082263));
#14129=CARTESIAN_POINT('Ctrl Pts',(-204.900988268614,62.4802052570581,10.6436672478278));
#14130=CARTESIAN_POINT('Ctrl Pts',(-204.067569447348,62.5129532579397,10.6966366874292));
#14131=CARTESIAN_POINT('Ctrl Pts',(-203.252008009052,63.0001619484835,10.7496061270306));
#14132=CARTESIAN_POINT('Ctrl Pts',(-202.82815275936,63.7184975876597,10.8025755666321));
#14133=CARTESIAN_POINT('Ctrl Pts',(-202.601856496319,64.1020168925947,10.8308559435907));
#14134=CARTESIAN_POINT('Ctrl Pts',(-202.487215718844,64.5514187197568,10.8591363205494));
#14135=CARTESIAN_POINT('Ctrl Pts',(-202.486473208904,65.0004666846809,10.8874166975081));
#14136=CARTESIAN_POINT('Ctrl Pts',(-202.481967556149,65.0022835844395,10.6125833024919));
#14137=CARTESIAN_POINT('Ctrl Pts',(-202.488050336832,64.3455973490155,10.5710385486894));
#14138=CARTESIAN_POINT('Ctrl Pts',(-202.751265847009,63.6845916284616,10.5294937948868));
#14139=CARTESIAN_POINT('Ctrl Pts',(-203.212768103735,63.220963415075,10.4879490410842));
#14140=CARTESIAN_POINT('Ctrl Pts',(-203.801182131406,62.6298387988791,10.4349796014828));
#14141=CARTESIAN_POINT('Ctrl Pts',(-204.711934572726,62.3595745208452,10.3820101618813));
#14142=CARTESIAN_POINT('Ctrl Pts',(-205.52754159824,62.5340582156802,10.3290407222799));
#14143=CARTESIAN_POINT('Ctrl Pts',(-206.343148623755,62.7085419105152,10.2760712826785));
#14144=CARTESIAN_POINT('Ctrl Pts',(-207.063610233464,63.327773578219,10.223101843077));
#14145=CARTESIAN_POINT('Ctrl Pts',(-207.358670851702,64.1079008828283,10.1701324034756));
#14146=CARTESIAN_POINT('Ctrl Pts',(-207.65373146994,64.8880281874377,10.1171629638742));
#14147=CARTESIAN_POINT('Ctrl Pts',(-207.523391096707,65.8290511289526,10.0641935242727));
#14148=CARTESIAN_POINT('Ctrl Pts',(-207.0273970307,66.4996100497921,10.0112240846713));
#14149=CARTESIAN_POINT('Ctrl Pts',(-206.531402964692,67.1701689706315,9.95825464506984));
#14150=CARTESIAN_POINT('Ctrl Pts',(-205.66975520591,67.5702638707955,9.90528520546841));
#14151=CARTESIAN_POINT('Ctrl Pts',(-204.837428271749,67.5164934839379,9.85231576586697));
#14152=CARTESIAN_POINT('Ctrl Pts',(-204.005101337589,67.4627230970802,9.79934632626553));
#14153=CARTESIAN_POINT('Ctrl Pts',(-203.20209522805,66.955087423201,9.7463768866641));
#14154=CARTESIAN_POINT('Ctrl Pts',(-202.796503456228,66.2262838183368,9.69340744706266));
#14155=CARTESIAN_POINT('Ctrl Pts',(-202.590210870358,65.8555988323875,9.66646606553909));
#14156=CARTESIAN_POINT('Ctrl Pts',(-202.486727607399,65.4276986856451,9.63952468401551));
#14157=CARTESIAN_POINT('Ctrl Pts',(-202.486546886373,64.9998805727156,9.61258330249194));
#14158=CARTESIAN_POINT('Origin',(-205.,65.,9.));
#14159=CARTESIAN_POINT('',(-202.48152822651,64.9977697676256,8.61258330249193));
#14160=CARTESIAN_POINT('',(-202.478564103745,65.0007934494835,8.88741669750805));
#14161=CARTESIAN_POINT('',(-202.4825,65.,9.));
#14162=CARTESIAN_POINT('Ctrl Pts',(-202.478564103745,65.0007934494835,8.88741669750805));
#14163=CARTESIAN_POINT('Ctrl Pts',(-202.478385247511,65.044156657915,8.89016971199883));
#14164=CARTESIAN_POINT('Ctrl Pts',(-202.479406854651,65.0875112638012,8.89292272648962));
#14165=CARTESIAN_POINT('Ctrl Pts',(-202.48165537137,65.130802144333,8.8956757409804));
#14166=CARTESIAN_POINT('Ctrl Pts',(-202.524918009827,65.9637413421835,8.94864518058183));
#14167=CARTESIAN_POINT('Ctrl Pts',(-203.02237980079,66.7730895579156,9.00161462018326));
#14168=CARTESIAN_POINT('Ctrl Pts',(-203.746007039296,67.1878460923965,9.0545840597847));
#14169=CARTESIAN_POINT('Ctrl Pts',(-204.469634277802,67.6026026268774,9.10755349938614));
#14170=CARTESIAN_POINT('Ctrl Pts',(-205.41942696385,67.6227674801071,9.16052293898758));
#14171=CARTESIAN_POINT('Ctrl Pts',(-206.160005437975,67.2390971960543,9.21349237858901));
#14172=CARTESIAN_POINT('Ctrl Pts',(-206.9005839121,66.8554269120015,9.26646181819045));
#14173=CARTESIAN_POINT('Ctrl Pts',(-207.431948174301,66.0679214906662,9.31943125779188));
#14174=CARTESIAN_POINT('Ctrl Pts',(-207.510523816259,65.2375690162959,9.37240069739331));
#14175=CARTESIAN_POINT('Ctrl Pts',(-207.589099458218,64.4072165419256,9.42537013699475));
#14176=CARTESIAN_POINT('Ctrl Pts',(-207.214886479934,63.5340170145203,9.47833957659619));
#14177=CARTESIAN_POINT('Ctrl Pts',(-206.559422019403,63.0182402176573,9.53130901619763));
#14178=CARTESIAN_POINT('Ctrl Pts',(-205.903957558871,62.5024634207942,9.58427845579906));
#14179=CARTESIAN_POINT('Ctrl Pts',(-204.967241616092,62.3441093544734,9.6372478954005));
#14180=CARTESIAN_POINT('Ctrl Pts',(-204.178659544495,62.615766637751,9.69021733500193));
#14181=CARTESIAN_POINT('Ctrl Pts',(-203.390077472898,62.8874239210286,9.74318677460337));
#14182=CARTESIAN_POINT('Ctrl Pts',(-202.749629272483,63.5890925539047,9.7961562142048));
#14183=CARTESIAN_POINT('Ctrl Pts',(-202.550892819242,64.3991315562713,9.84912565380624));
#14184=CARTESIAN_POINT('Ctrl Pts',(-202.503004664151,64.5943210785895,9.86188933504018));
#14185=CARTESIAN_POINT('Ctrl Pts',(-202.480763716917,64.7958029338822,9.87465301627412));
#14186=CARTESIAN_POINT('Ctrl Pts',(-202.482611670102,64.997686958861,9.88741669750806));
#14187=CARTESIAN_POINT('Ctrl Pts',(-202.486546886373,64.9998805727156,9.61258330249194));
#14188=CARTESIAN_POINT('Ctrl Pts',(-202.486372291861,64.5865656623298,9.58655524441408));
#14189=CARTESIAN_POINT('Ctrl Pts',(-202.582614964632,64.1733273180761,9.56052718633622));
#14190=CARTESIAN_POINT('Ctrl Pts',(-202.775719644012,63.8118308540053,9.53449912825836));
#14191=CARTESIAN_POINT('Ctrl Pts',(-203.16870503772,63.0761530303869,9.48152968865693));
#14192=CARTESIAN_POINT('Ctrl Pts',(-203.962853259241,62.554768918999,9.42856024905549));
#14193=CARTESIAN_POINT('Ctrl Pts',(-204.794131201844,62.4866780828008,9.37559080945405));
#14194=CARTESIAN_POINT('Ctrl Pts',(-205.625409144447,62.4185872466025,9.32262136985262));
#14195=CARTESIAN_POINT('Ctrl Pts',(-206.493816808132,62.8037896855938,9.26965193025118));
#14196=CARTESIAN_POINT('Ctrl Pts',(-207.001280972872,63.4657107544051,9.21668249064975));
#14197=CARTESIAN_POINT('Ctrl Pts',(-207.508745137613,64.1276318232163,9.16371305104831));
#14198=CARTESIAN_POINT('Ctrl Pts',(-207.655265803409,65.0662715218476,9.11074361144688));
#14199=CARTESIAN_POINT('Ctrl Pts',(-207.373678715875,65.8513626579371,9.05777417184544));
#14200=CARTESIAN_POINT('Ctrl Pts',(-207.092091628341,66.6364537940267,9.004804732244));
#14201=CARTESIAN_POINT('Ctrl Pts',(-206.382396787478,67.2679963675745,8.95183529264257));
#14202=CARTESIAN_POINT('Ctrl Pts',(-205.56991434228,67.4564947921768,8.89886585304113));
#14203=CARTESIAN_POINT('Ctrl Pts',(-204.757431897082,67.644993216779,8.8458964134397));
#14204=CARTESIAN_POINT('Ctrl Pts',(-203.84216184755,67.3904474924357,8.79292697383826));
#14205=CARTESIAN_POINT('Ctrl Pts',(-203.243658869497,66.8095399566832,8.73995753423683));
#14206=CARTESIAN_POINT('Ctrl Pts',(-202.763924028678,66.3439088831306,8.69749945698853));
#14207=CARTESIAN_POINT('Ctrl Pts',(-202.48771051161,65.6685919114507,8.65504137974023));
#14208=CARTESIAN_POINT('Ctrl Pts',(-202.48152822651,64.9977697676256,8.61258330249193));
#14209=CARTESIAN_POINT('Origin',(-205.,65.,9.));
#14210=CARTESIAN_POINT('',(-202.479185657883,65.0013671530438,7.61258330249194));
#14211=CARTESIAN_POINT('',(-202.484985693937,65.0018590734507,7.88741669750805));
#14212=CARTESIAN_POINT('',(-202.4825,65.,9.));
#14213=CARTESIAN_POINT('Ctrl Pts',(-202.484985693937,65.0018590734507,7.88741669750805));
#14214=CARTESIAN_POINT('Ctrl Pts',(-202.483005747609,65.2915238451685,7.90568640772355));
#14215=CARTESIAN_POINT('Ctrl Pts',(-202.529199000709,65.5805765589219,7.92395611793905));
#14216=CARTESIAN_POINT('Ctrl Pts',(-202.626321312497,65.851362647761,7.94222582815455));
#14217=CARTESIAN_POINT('Ctrl Pts',(-202.907908396665,66.6364537744666,7.99519526775599));
#14218=CARTESIAN_POINT('Ctrl Pts',(-203.617603229046,67.2679963404659,8.04816470735743));
#14219=CARTESIAN_POINT('Ctrl Pts',(-204.430085664532,67.4564947628151,8.10113414695886));
#14220=CARTESIAN_POINT('Ctrl Pts',(-205.242568100018,67.6449931851643,8.1541035865603));
#14221=CARTESIAN_POINT('Ctrl Pts',(-206.15783813861,67.3904474638634,8.20707302616174));
#14222=CARTESIAN_POINT('Ctrl Pts',(-206.756341109509,66.8095399350544,8.26004246576317));
#14223=CARTESIAN_POINT('Ctrl Pts',(-207.354844080409,66.2286324062453,8.3130119053646));
#14224=CARTESIAN_POINT('Ctrl Pts',(-207.636579983615,65.3213630699281,8.36598134496604));
#14225=CARTESIAN_POINT('Ctrl Pts',(-207.47240265555,64.5036191196896,8.41895078456747));
#14226=CARTESIAN_POINT('Ctrl Pts',(-207.308225327486,63.6858751694511,8.47192022416891));
#14227=CARTESIAN_POINT('Ctrl Pts',(-206.69813476815,62.9576566052913,8.52488966377034));
#14228=CARTESIAN_POINT('Ctrl Pts',(-205.921793080516,62.6527747474469,8.57785910337178));
#14229=CARTESIAN_POINT('Ctrl Pts',(-205.145451392881,62.3478928896025,8.63082854297322));
#14230=CARTESIAN_POINT('Ctrl Pts',(-204.202858576947,62.4663477380736,8.68379798257465));
#14231=CARTESIAN_POINT('Ctrl Pts',(-203.526093911955,62.9538402522936,8.73676742217609));
#14232=CARTESIAN_POINT('Ctrl Pts',(-202.884503168825,63.4159960069425,8.78698384728674));
#14233=CARTESIAN_POINT('Ctrl Pts',(-202.481826535046,64.2098258334208,8.8372002723974));
#14234=CARTESIAN_POINT('Ctrl Pts',(-202.478564103745,65.0007934494835,8.88741669750805));
#14235=CARTESIAN_POINT('Ctrl Pts',(-202.48152822651,64.9977697676256,8.61258330249193));
#14236=CARTESIAN_POINT('Ctrl Pts',(-202.479997675833,64.831694074018,8.60207194013879));
#14237=CARTESIAN_POINT('Ctrl Pts',(-202.495017634632,64.6658938733246,8.59156057778566));
#14238=CARTESIAN_POINT('Ctrl Pts',(-202.527597314898,64.5036191137564,8.58104921543252));
#14239=CARTESIAN_POINT('Ctrl Pts',(-202.691774644925,63.6858751537437,8.52807977583108));
#14240=CARTESIAN_POINT('Ctrl Pts',(-203.301865211552,62.9576565808797,8.47511033622965));
#14241=CARTESIAN_POINT('Ctrl Pts',(-204.078206908466,62.6527747193912,8.42214089662821));
#14242=CARTESIAN_POINT('Ctrl Pts',(-204.85454860538,62.3478928579027,8.36917145702678));
#14243=CARTESIAN_POINT('Ctrl Pts',(-205.797141432581,62.4663477077896,8.31620201742534));
#14244=CARTESIAN_POINT('Ctrl Pts',(-206.473906105662,62.9538402278365,8.2632325778239));
#14245=CARTESIAN_POINT('Ctrl Pts',(-207.150670778743,63.4413327478833,8.21026313822247));
#14246=CARTESIAN_POINT('Ctrl Pts',(-207.561607297705,64.2978629380902,8.15729369862104));
#14247=CARTESIAN_POINT('Ctrl Pts',(-207.518344658731,65.1308021458965,8.1043242590196));
#14248=CARTESIAN_POINT('Ctrl Pts',(-207.475082019757,65.9637413537029,8.05135481941817));
#14249=CARTESIAN_POINT('Ctrl Pts',(-206.977620222847,66.7730895791089,7.99838537981673));
#14250=CARTESIAN_POINT('Ctrl Pts',(-206.253992975692,67.1878461185472,7.94541594021529));
#14251=CARTESIAN_POINT('Ctrl Pts',(-205.530365728537,67.6026026579855,7.89244650061386));
#14252=CARTESIAN_POINT('Ctrl Pts',(-204.580573031136,67.6227675114562,7.83947706101243));
#14253=CARTESIAN_POINT('Ctrl Pts',(-203.83999454816,67.2390972228175,7.78650762141099));
#14254=CARTESIAN_POINT('Ctrl Pts',(-203.099416065183,66.8554269341788,7.73353818180956));
#14255=CARTESIAN_POINT('Ctrl Pts',(-202.568051796631,66.0679215034307,7.68056874220812));
#14256=CARTESIAN_POINT('Ctrl Pts',(-202.489476153733,65.2375690191355,7.62759930260668));
#14257=CARTESIAN_POINT('Ctrl Pts',(-202.482051168863,65.159105077831,7.6225939692351));
#14258=CARTESIAN_POINT('Ctrl Pts',(-202.478669249412,65.0802585442292,7.61758863586352));
#14259=CARTESIAN_POINT('Ctrl Pts',(-202.479185657883,65.0013671530438,7.61258330249194));
#14260=CARTESIAN_POINT('Origin',(-205.,65.,9.));
#14261=CARTESIAN_POINT('',(-202.485705065293,65.0014474068846,6.61258330249194));
#14262=CARTESIAN_POINT('',(-202.485300168502,64.9982947807633,6.88741669750805));
#14263=CARTESIAN_POINT('',(-202.4825,65.,9.));
#14264=CARTESIAN_POINT('Ctrl Pts',(-202.485300168502,64.9982947807633,6.88741669750805));
#14265=CARTESIAN_POINT('Ctrl Pts',(-202.488632032345,65.5341438421791,6.92120310344827));
#14266=CARTESIAN_POINT('Ctrl Pts',(-202.656234597268,66.071895942272,6.9549895093885));
#14267=CARTESIAN_POINT('Ctrl Pts',(-202.972602993533,66.4996100318676,6.98877591532872));
#14268=CARTESIAN_POINT('Ctrl Pts',(-203.468597053612,67.1701689446921,7.04174535493015));
#14269=CARTESIAN_POINT('Ctrl Pts',(-204.330244802095,67.5702638400739,7.09471479453159));
#14270=CARTESIAN_POINT('Ctrl Pts',(-205.162571726307,67.516493453859,7.14768423413302));
#14271=CARTESIAN_POINT('Ctrl Pts',(-205.99489865052,67.4627230676441,7.20065367373446));
#14272=CARTESIAN_POINT('Ctrl Pts',(-206.79790475046,66.9550873998325,7.25362311333589));
#14273=CARTESIAN_POINT('Ctrl Pts',(-207.203496517434,66.2262838036795,7.30659255293733));
#14274=CARTESIAN_POINT('Ctrl Pts',(-207.609088284407,65.4974802075266,7.35956199253877));
#14275=CARTESIAN_POINT('Ctrl Pts',(-207.617265718413,64.5475086830323,7.4125314321402));
#14276=CARTESIAN_POINT('Ctrl Pts',(-207.224280329402,63.8118308682072,7.46550087174164));
#14277=CARTESIAN_POINT('Ctrl Pts',(-206.831294940391,63.0761530533821,7.51847031134307));
#14278=CARTESIAN_POINT('Ctrl Pts',(-206.037146728362,62.5547689482262,7.57143975094451));
#14279=CARTESIAN_POINT('Ctrl Pts',(-205.205868795696,62.4866781128418,7.62440919054594));
#14280=CARTESIAN_POINT('Ctrl Pts',(-204.374590863029,62.4185872774574,7.67737863014738));
#14281=CARTESIAN_POINT('Ctrl Pts',(-203.506183209724,62.8037897118444,7.73034806974881));
#14282=CARTESIAN_POINT('Ctrl Pts',(-202.998719051049,63.4657107727439,7.78331750935025));
#14283=CARTESIAN_POINT('Ctrl Pts',(-202.666284554637,63.8993283805738,7.81801723873618));
#14284=CARTESIAN_POINT('Ctrl Pts',(-202.48874621345,64.4516976821268,7.85271696812212));
#14285=CARTESIAN_POINT('Ctrl Pts',(-202.484985693937,65.0018590734507,7.88741669750805));
#14286=CARTESIAN_POINT('Ctrl Pts',(-202.479185657883,65.0013671530438,7.61258330249194));
#14287=CARTESIAN_POINT('Ctrl Pts',(-202.48413419356,64.2453825289387,7.56461919626208));
#14288=CARTESIAN_POINT('Ctrl Pts',(-202.847051437472,63.4852788025991,7.51665509003223));
#14289=CARTESIAN_POINT('Ctrl Pts',(-203.440577961958,63.0182401939698,7.46869098380237));
#14290=CARTESIAN_POINT('Ctrl Pts',(-204.096042430324,62.5024633909419,7.41572154420094));
#14291=CARTESIAN_POINT('Ctrl Pts',(-205.032758384299,62.3441093227284,7.3627521045995));
#14292=CARTESIAN_POINT('Ctrl Pts',(-205.821340465322,62.615766609253,7.30978266499807));
#14293=CARTESIAN_POINT('Ctrl Pts',(-206.609922546345,62.8874238957777,7.25681322539663));
#14294=CARTESIAN_POINT('Ctrl Pts',(-207.250370754415,63.5890925370406,7.2038437857952));
#14295=CARTESIAN_POINT('Ctrl Pts',(-207.449107210032,64.3991315490894,7.15087434619376));
#14296=CARTESIAN_POINT('Ctrl Pts',(-207.647843665648,65.2091705611382,7.09790490659232));
#14297=CARTESIAN_POINT('Ctrl Pts',(-207.404868368812,66.127579943973,7.04493546699089));
#14298=CARTESIAN_POINT('Ctrl Pts',(-206.831559837749,66.7333659689382,6.99196602738945));
#14299=CARTESIAN_POINT('Ctrl Pts',(-206.258251306687,67.3391519939033,6.93899658778802));
#14300=CARTESIAN_POINT('Ctrl Pts',(-205.354609541398,67.6323146609989,6.88602714818658));
#14301=CARTESIAN_POINT('Ctrl Pts',(-204.534858877184,67.4784698419375,6.83305770858515));
#14302=CARTESIAN_POINT('Ctrl Pts',(-203.715108212969,67.3246250228761,6.78008826898371));
#14303=CARTESIAN_POINT('Ctrl Pts',(-202.979248649829,66.7237727176577,6.72711882938228));
#14304=CARTESIAN_POINT('Ctrl Pts',(-202.66459409923,65.9513402651935,6.67414938978084));
#14305=CARTESIAN_POINT('Ctrl Pts',(-202.542687016746,65.6520756064832,6.65362736068454));
#14306=CARTESIAN_POINT('Ctrl Pts',(-202.48400413857,65.3270562251041,6.63310533158824));
#14307=CARTESIAN_POINT('Ctrl Pts',(-202.485705065293,65.0014474068846,6.61258330249194));
#14308=CARTESIAN_POINT('Origin',(-205.,65.,9.));
#14309=CARTESIAN_POINT('',(-202.484474821952,64.9979518749283,5.61258330249194));
#14310=CARTESIAN_POINT('',(-202.478781766938,64.9989624751798,5.88741669750806));
#14311=CARTESIAN_POINT('',(-202.4825,65.,9.));
#14312=CARTESIAN_POINT('Ctrl Pts',(-202.478781766938,64.9989624751798,5.88741669750806));
#14313=CARTESIAN_POINT('Ctrl Pts',(-202.482826134015,65.7757224753788,5.936719799173));
#14314=CARTESIAN_POINT('Ctrl Pts',(-202.869070859878,66.5559564232876,5.98602290083794));
#14315=CARTESIAN_POINT('Ctrl Pts',(-203.491087909026,67.0204834003828,6.03532600250288));
#14316=CARTESIAN_POINT('Ctrl Pts',(-204.159360155665,67.5195541043661,6.08829544210431));
#14317=CARTESIAN_POINT('Ctrl Pts',(-205.099774104093,67.6542180319002,6.14126488170575));
#14318=CARTESIAN_POINT('Ctrl Pts',(-205.881249255757,67.3627459911589,6.19423432130718));
#14319=CARTESIAN_POINT('Ctrl Pts',(-206.662724407421,67.0712739504177,6.24720376090862));
#14320=CARTESIAN_POINT('Ctrl Pts',(-207.285260762321,66.353665941401,6.30017320051005));
#14321=CARTESIAN_POINT('Ctrl Pts',(-207.463491134351,65.538869465164,6.35314264011149));
#14322=CARTESIAN_POINT('Ctrl Pts',(-207.64172150638,64.724072988927,6.40611207971293));
#14323=CARTESIAN_POINT('Ctrl Pts',(-207.37564589554,63.8120880454697,6.45908151931436));
#14324=CARTESIAN_POINT('Ctrl Pts',(-206.787231874903,63.2209634363394,6.5120509589158));
#14325=CARTESIAN_POINT('Ctrl Pts',(-206.198817854265,62.6298388272089,6.56502039851723));
#14326=CARTESIAN_POINT('Ctrl Pts',(-205.288065423831,62.3595745524054,6.61798983811866));
#14327=CARTESIAN_POINT('Ctrl Pts',(-204.472458408065,62.5340582451549,6.6709592777201));
#14328=CARTESIAN_POINT('Ctrl Pts',(-203.656851392299,62.7085419379043,6.72392871732154));
#14329=CARTESIAN_POINT('Ctrl Pts',(-202.936389791202,63.3277735982066,6.77689815692298));
#14330=CARTESIAN_POINT('Ctrl Pts',(-202.64132917649,64.1079008934913,6.82986759652441));
#14331=CARTESIAN_POINT('Ctrl Pts',(-202.534472133133,64.3904262190013,6.84905063018563));
#14332=CARTESIAN_POINT('Ctrl Pts',(-202.483408423747,64.6940537614417,6.86823366384684));
#14333=CARTESIAN_POINT('Ctrl Pts',(-202.485300168502,64.9982947807633,6.88741669750805));
#14334=CARTESIAN_POINT('Ctrl Pts',(-202.485705065293,65.0014474068846,6.61258330249194));
#14335=CARTESIAN_POINT('Ctrl Pts',(-202.488394403048,64.4866268236333,6.5801358919868));
#14336=CARTESIAN_POINT('Ctrl Pts',(-202.642036120458,63.9703327179061,6.54768848148167));
#14337=CARTESIAN_POINT('Ctrl Pts',(-202.935403348754,63.5520325662536,6.51524107097653));
#14338=CARTESIAN_POINT('Ctrl Pts',(-203.414316686931,62.869169919488,6.4622716313751));
#14339=CARTESIAN_POINT('Ctrl Pts',(-204.265592901342,62.4474572256667,6.40930219177367));
#14340=CARTESIAN_POINT('Ctrl Pts',(-205.099011732569,62.4802052269398,6.35633275217223));
#14341=CARTESIAN_POINT('Ctrl Pts',(-205.932430563797,62.5129532282128,6.30336331257079));
#14342=CARTESIAN_POINT('Ctrl Pts',(-206.747992011841,63.0001619245801,6.25039387296935));
#14343=CARTESIAN_POINT('Ctrl Pts',(-207.1718472666,63.7184975723424,6.19742443336792));
#14344=CARTESIAN_POINT('Ctrl Pts',(-207.595702521358,64.4368332201046,6.14445499376648));
#14345=CARTESIAN_POINT('Ctrl Pts',(-207.62785158283,65.3862958192617,6.09148555416505));
#14346=CARTESIAN_POINT('Ctrl Pts',(-207.253557500899,66.1316570203338,6.03851611456362));
#14347=CARTESIAN_POINT('Ctrl Pts',(-206.879263418968,66.8770182214058,5.98554667496218));
#14348=CARTESIAN_POINT('Ctrl Pts',(-206.098526193634,67.4182780243928,5.93257723536074));
#14349=CARTESIAN_POINT('Ctrl Pts',(-205.26923140592,67.5073259603798,5.87960779575931));
#14350=CARTESIAN_POINT('Ctrl Pts',(-204.439936618207,67.5963738963668,5.82663835615787));
#14351=CARTESIAN_POINT('Ctrl Pts',(-203.562084268114,67.2332099653539,5.77366891655643));
#14352=CARTESIAN_POINT('Ctrl Pts',(-203.038076967138,66.5843064838134,5.720699476955));
#14353=CARTESIAN_POINT('Ctrl Pts',(-202.681559037815,66.1428131589339,5.68466075213398));
#14354=CARTESIAN_POINT('Ctrl Pts',(-202.488836318919,65.5690507238242,5.64862202731296));
#14355=CARTESIAN_POINT('Ctrl Pts',(-202.484474821952,64.9979518749283,5.61258330249194));
#14356=CARTESIAN_POINT('Origin',(-205.,65.,9.));
#14357=CARTESIAN_POINT('',(-202.478344473785,64.9995851075454,4.61258330249193));
#14358=CARTESIAN_POINT('',(-202.48217288036,65.0022992261759,4.88741669750805));
#14359=CARTESIAN_POINT('',(-202.4825,65.,9.));
#14360=CARTESIAN_POINT('Ctrl Pts',(-202.48217288036,65.0022992261759,4.88741669750805));
#14361=CARTESIAN_POINT('Ctrl Pts',(-202.480439771035,65.1896536409608,4.89926705529628));
#14362=CARTESIAN_POINT('Ctrl Pts',(-202.499576724591,65.3766572882651,4.9111174130845));
#14363=CARTESIAN_POINT('Ctrl Pts',(-202.540911860868,65.5586182896119,4.92296777087273));
#14364=CARTESIAN_POINT('Ctrl Pts',(-202.725674130799,66.3719584809291,4.97593721047417));
#14365=CARTESIAN_POINT('Ctrl Pts',(-203.353948275965,67.0845483814278,5.0289066500756));
#14366=CARTESIAN_POINT('Ctrl Pts',(-204.137736939267,67.3697407629541,5.08187608967704));
#14367=CARTESIAN_POINT('Ctrl Pts',(-204.92152560257,67.6549331444803,5.13484552927847));
#14368=CARTESIAN_POINT('Ctrl Pts',(-205.860828784009,67.5127280070342,5.18781496887991));
#14369=CARTESIAN_POINT('Ctrl Pts',(-206.525075154411,67.0083113909224,5.24078440848134));
#14370=CARTESIAN_POINT('Ctrl Pts',(-207.189321524813,66.5038947748106,5.29375384808278));
#14371=CARTESIAN_POINT('Ctrl Pts',(-207.578511084179,65.6372666800331,5.34672328768421));
#14372=CARTESIAN_POINT('Ctrl Pts',(-207.51424151344,64.8056845821744,5.39969272728565));
#14373=CARTESIAN_POINT('Ctrl Pts',(-207.449971942702,63.9741024843156,5.45266216688709));
#14374=CARTESIAN_POINT('Ctrl Pts',(-206.932243241859,63.1775663833756,5.50563160648852));
#14375=CARTESIAN_POINT('Ctrl Pts',(-206.198379354105,62.7812039766656,5.55860104608996));
#14376=CARTESIAN_POINT('Ctrl Pts',(-205.464515466351,62.3848415699556,5.61157048569139));
#14377=CARTESIAN_POINT('Ctrl Pts',(-204.514516391686,62.3886528574756,5.66453992529283));
#14378=CARTESIAN_POINT('Ctrl Pts',(-203.783856396965,62.7908907663254,5.71750936489426));
#14379=CARTESIAN_POINT('Ctrl Pts',(-203.053196402243,63.1931286751752,5.7704788044957));
#14380=CARTESIAN_POINT('Ctrl Pts',(-202.541875487466,63.9937932053548,5.82344824409714));
#14381=CARTESIAN_POINT('Ctrl Pts',(-202.484280302502,64.8258642106609,5.87641768369857));
#14382=CARTESIAN_POINT('Ctrl Pts',(-202.48029378852,64.8834569191276,5.88008402163507));
#14383=CARTESIAN_POINT('Ctrl Pts',(-202.478481014735,64.9412000918792,5.88375035957156));
#14384=CARTESIAN_POINT('Ctrl Pts',(-202.478781766938,64.9989624751798,5.88741669750806));
#14385=CARTESIAN_POINT('Ctrl Pts',(-202.484474821952,64.9979518749283,5.61258330249194));
#14386=CARTESIAN_POINT('Ctrl Pts',(-202.482425824339,64.7296540433568,5.59565258771152));
#14387=CARTESIAN_POINT('Ctrl Pts',(-202.521949050352,64.4619440780171,5.57872187293111));
#14388=CARTESIAN_POINT('Ctrl Pts',(-202.605591636875,64.208812530353,5.5617911581507));
#14389=CARTESIAN_POINT('Ctrl Pts',(-202.86727585945,63.4168650905012,5.50882171854926));
#14390=CARTESIAN_POINT('Ctrl Pts',(-203.560806556459,62.7676132428658,5.45585227894782));
#14391=CARTESIAN_POINT('Ctrl Pts',(-204.368273132118,62.5586704061261,5.40288283934639));
#14392=CARTESIAN_POINT('Ctrl Pts',(-205.175739707778,62.3497275693864,5.34991339974495));
#14393=CARTESIAN_POINT('Ctrl Pts',(-206.097142162087,62.5810937435424,5.29694396014351));
#14394=CARTESIAN_POINT('Ctrl Pts',(-206.710114759154,63.1467119673268,5.24397452054208));
#14395=CARTESIAN_POINT('Ctrl Pts',(-207.323087356221,63.7123301911111,5.19100508094064));
#14396=CARTESIAN_POINT('Ctrl Pts',(-207.627630096046,64.6122004645237,5.13803564133921));
#14397=CARTESIAN_POINT('Ctrl Pts',(-207.484142288597,65.4338272830649,5.08506620173777));
#14398=CARTESIAN_POINT('Ctrl Pts',(-207.340654481149,66.255454101606,5.03209676213634));
#14399=CARTESIAN_POINT('Ctrl Pts',(-206.749136126427,66.9988374652756,4.9791273225349));
#14400=CARTESIAN_POINT('Ctrl Pts',(-205.980735932599,67.3232145944874,4.92615788293347));
#14401=CARTESIAN_POINT('Ctrl Pts',(-205.21233573877,67.6475917236993,4.87318844333203));
#14402=CARTESIAN_POINT('Ctrl Pts',(-204.267053705834,67.5529626184535,4.82021900373059));
#14403=CARTESIAN_POINT('Ctrl Pts',(-203.578201835077,67.082704731772,4.76724956412916));
#14404=CARTESIAN_POINT('Ctrl Pts',(-202.907738863261,66.6250003781818,4.71569414358342));
#14405=CARTESIAN_POINT('Ctrl Pts',(-202.48019798657,65.811454380222,4.66413872303768));
#14406=CARTESIAN_POINT('Ctrl Pts',(-202.478344473785,64.9995851075454,4.61258330249193));
#14407=CARTESIAN_POINT('Origin',(-205.,65.,9.));
#14408=CARTESIAN_POINT('',(-202.483242841669,65.0022852126429,3.61258330249194));
#14409=CARTESIAN_POINT('',(-202.486532959272,64.9997695214146,3.88741669750805));
#14410=CARTESIAN_POINT('',(-202.4825,65.,9.));
#14411=CARTESIAN_POINT('Ctrl Pts',(-202.486532959272,64.9997695214146,3.88741669750805));
#14412=CARTESIAN_POINT('Ctrl Pts',(-202.486887346168,65.4343411087312,3.914783751021));
#14413=CARTESIAN_POINT('Ctrl Pts',(-202.593847191985,65.8690761086745,3.94215080453394));
#14414=CARTESIAN_POINT('Ctrl Pts',(-202.80641367505,66.2439243966071,3.96951785804689));
#14415=CARTESIAN_POINT('Ctrl Pts',(-203.217840045108,66.9694502095321,4.02248729764833));
#14416=CARTESIAN_POINT('Ctrl Pts',(-204.024893383128,67.4706265032263,4.07545673724976));
#14417=CARTESIAN_POINT('Ctrl Pts',(-204.857624949113,67.517716865417,4.12842617685119));
#14418=CARTESIAN_POINT('Ctrl Pts',(-205.690356515098,67.5648072276077,4.18139561645263));
#14419=CARTESIAN_POINT('Ctrl Pts',(-206.548766309047,67.1578116582949,4.23436505605407));
#14420=CARTESIAN_POINT('Ctrl Pts',(-207.03936407854,66.4832946520063,4.2873344956555));
#14421=CARTESIAN_POINT('Ctrl Pts',(-207.529961848034,65.8087776457177,4.34030393525694));
#14422=CARTESIAN_POINT('Ctrl Pts',(-207.652747593072,64.8667392024533,4.39327337485837));
#14423=CARTESIAN_POINT('Ctrl Pts',(-207.351437014309,64.0890044801174,4.44624281445981));
#14424=CARTESIAN_POINT('Ctrl Pts',(-207.050126435545,63.3112697577815,4.49921225406124));
#14425=CARTESIAN_POINT('Ctrl Pts',(-206.32471953298,62.6978387563742,4.55218169366268));
#14426=CARTESIAN_POINT('Ctrl Pts',(-205.507738776886,62.5299048188465,4.60515113326412));
#14427=CARTESIAN_POINT('Ctrl Pts',(-204.690758020792,62.3619708813189,4.65812057286555));
#14428=CARTESIAN_POINT('Ctrl Pts',(-203.782203411168,62.639534007671,4.71109001246699));
#14429=CARTESIAN_POINT('Ctrl Pts',(-203.198551303705,63.2353608119149,4.76405945206842));
#14430=CARTESIAN_POINT('Ctrl Pts',(-202.745474228738,63.6978888525088,4.80517853388163));
#14431=CARTESIAN_POINT('Ctrl Pts',(-202.488186526988,64.3522056469539,4.84629761569484));
#14432=CARTESIAN_POINT('Ctrl Pts',(-202.48217288036,65.0022992261759,4.88741669750805));
#14433=CARTESIAN_POINT('Ctrl Pts',(-202.478344473785,64.9995851075454,4.61258330249193));
#14434=CARTESIAN_POINT('Ctrl Pts',(-202.478293637183,64.9773178345769,4.61116928343624));
#14435=CARTESIAN_POINT('Ctrl Pts',(-202.47856302365,64.955051822924,4.60975526438055));
#14436=CARTESIAN_POINT('Ctrl Pts',(-202.479156404012,64.9327944489305,4.60834124532485));
#14437=CARTESIAN_POINT('Ctrl Pts',(-202.501384552282,64.0990287208875,4.55537180572342));
#14438=CARTESIAN_POINT('Ctrl Pts',(-202.9782625574,63.2773839329187,4.50240236612198));
#14439=CARTESIAN_POINT('Ctrl Pts',(-203.691192206802,62.8444974641621,4.44943292652054));
#14440=CARTESIAN_POINT('Ctrl Pts',(-204.404121856204,62.4116109954056,4.39646348691911));
#14441=CARTESIAN_POINT('Ctrl Pts',(-205.353103149889,62.3674828458613,4.34349404731767));
#14442=CARTESIAN_POINT('Ctrl Pts',(-206.10312836612,62.7323411126537,4.29052460771624));
#14443=CARTESIAN_POINT('Ctrl Pts',(-206.853153582352,63.0971993794462,4.23755516811481));
#14444=CARTESIAN_POINT('Ctrl Pts',(-207.404222721129,63.8710440625754,4.18458572851337));
#14445=CARTESIAN_POINT('Ctrl Pts',(-207.503728768821,64.6991490838892,4.13161628891193));
#14446=CARTESIAN_POINT('Ctrl Pts',(-207.603234816513,65.5272541052031,4.0786468493105));
#14447=CARTESIAN_POINT('Ctrl Pts',(-207.251177773121,66.4096194647016,4.02567740970906));
#14448=CARTESIAN_POINT('Ctrl Pts',(-206.608938619917,66.941773812509,3.97270797010763));
#14449=CARTESIAN_POINT('Ctrl Pts',(-205.966699466714,67.4739281603165,3.91973853050619));
#14450=CARTESIAN_POINT('Ctrl Pts',(-205.034278203699,67.6558714964329,3.86676909090476));
#14451=CARTESIAN_POINT('Ctrl Pts',(-204.239091527064,67.4042020125377,3.81379965130332));
#14452=CARTESIAN_POINT('Ctrl Pts',(-203.44390485043,67.1525325286424,3.76083021170188));
#14453=CARTESIAN_POINT('Ctrl Pts',(-202.785952760175,66.4672502247354,3.70786077210045));
#14454=CARTESIAN_POINT('Ctrl Pts',(-202.566836817648,65.6624846789204,3.65489133249901));
#14455=CARTESIAN_POINT('Ctrl Pts',(-202.508499004114,65.4482224859956,3.64078865582999));
#14456=CARTESIAN_POINT('Ctrl Pts',(-202.481267947496,65.2254907625162,3.62668597916096));
#14457=CARTESIAN_POINT('Ctrl Pts',(-202.483242841669,65.0022852126429,3.61258330249194));
#14458=CARTESIAN_POINT('Origin',(-205.,65.,9.));
#14459=CARTESIAN_POINT('',(-202.486313063014,64.9991964084992,2.61258330249194));
#14460=CARTESIAN_POINT('',(-202.481325106597,64.9978038277911,2.88741669750805));
#14461=CARTESIAN_POINT('',(-202.4825,65.,9.));
#14462=CARTESIAN_POINT('Ctrl Pts',(-202.481325106597,64.9978038277911,2.88741669750805));
#14463=CARTESIAN_POINT('Ctrl Pts',(-202.487529301803,65.6752106759204,2.93030044674572));
#14464=CARTESIAN_POINT('Ctrl Pts',(-202.769932098234,66.3571775427947,2.97318419598338));
#14465=CARTESIAN_POINT('Ctrl Pts',(-203.258234527699,66.8235739378454,3.01606794522105));
#14466=CARTESIAN_POINT('Ctrl Pts',(-203.861379227138,67.3996605934466,3.06903738482248));
#14467=CARTESIAN_POINT('Ctrl Pts',(-204.778662186319,67.6468543225643,3.12200682442392));
#14468=CARTESIAN_POINT('Ctrl Pts',(-205.589606024052,67.4518429000389,3.17497626402536));
#14469=CARTESIAN_POINT('Ctrl Pts',(-206.400549861785,67.2568314775134,3.22794570362679));
#14470=CARTESIAN_POINT('Ctrl Pts',(-207.10515457807,66.6196149033449,3.28091514322823));
#14471=CARTESIAN_POINT('Ctrl Pts',(-207.38043330801,65.8322896946712,3.33388458282966));
#14472=CARTESIAN_POINT('Ctrl Pts',(-207.65571203795,65.0449644859974,3.3868540224311));
#14473=CARTESIAN_POINT('Ctrl Pts',(-207.501664781545,64.1075306428185,3.43982346203253));
#14474=CARTESIAN_POINT('Ctrl Pts',(-206.988905940528,63.4497025998243,3.49279290163397));
#14475=CARTESIAN_POINT('Ctrl Pts',(-206.47614709951,62.7918745568302,3.5457623412354));
#14476=CARTESIAN_POINT('Ctrl Pts',(-205.604676673879,62.413652314021,3.59873178083684));
#14477=CARTESIAN_POINT('Ctrl Pts',(-204.77397183649,62.4884108339761,3.65170122043828));
#14478=CARTESIAN_POINT('Ctrl Pts',(-203.9432669991,62.5631693539311,3.70467066003971));
#14479=CARTESIAN_POINT('Ctrl Pts',(-203.153327749952,63.0909086366506,3.75764009964115));
#14480=CARTESIAN_POINT('Ctrl Pts',(-202.766257826425,63.8297159440883,3.81060953924258));
#14481=CARTESIAN_POINT('Ctrl Pts',(-202.579170447364,64.1868129810278,3.83621192533107));
#14482=CARTESIAN_POINT('Ctrl Pts',(-202.486201423758,64.5932197422685,3.86181431141956));
#14483=CARTESIAN_POINT('Ctrl Pts',(-202.486532959272,64.9997695214146,3.88741669750805));
#14484=CARTESIAN_POINT('Ctrl Pts',(-202.483242841669,65.0022852126429,3.61258330249194));
#14485=CARTESIAN_POINT('Ctrl Pts',(-202.488685620045,64.3871341036922,3.57371653955953));
#14486=CARTESIAN_POINT('Ctrl Pts',(-202.715960806614,63.7683840689348,3.53484977662712));
#14487=CARTESIAN_POINT('Ctrl Pts',(-203.12527891892,63.313408795753,3.49598301369471));
#14488=CARTESIAN_POINT('Ctrl Pts',(-203.68311675752,62.6933472461235,3.44301357409327));
#14489=CARTESIAN_POINT('Ctrl Pts',(-204.57907222952,62.3774729345875,3.39004413449183));
#14490=CARTESIAN_POINT('Ctrl Pts',(-205.402444353812,62.5105808787203,3.3370746948904));
#14491=CARTESIAN_POINT('Ctrl Pts',(-206.225816478105,62.6436888228531,3.28410525528896));
#14492=CARTESIAN_POINT('Ctrl Pts',(-206.976605254691,63.2257790226548,3.23113581568753));
#14493=CARTESIAN_POINT('Ctrl Pts',(-207.310653303464,63.9900245867847,3.17816637608609));
#14494=CARTESIAN_POINT('Ctrl Pts',(-207.644701352236,64.7542701509147,3.12519693648466));
#14495=CARTESIAN_POINT('Ctrl Pts',(-207.562008673197,65.7006710793728,3.07222749688322));
#14496=CARTESIAN_POINT('Ctrl Pts',(-207.100481129582,66.3954024686292,3.01925805728179));
#14497=CARTESIAN_POINT('Ctrl Pts',(-206.638953585967,67.0901338578856,2.96628861768035));
#14498=CARTESIAN_POINT('Ctrl Pts',(-205.798591177777,67.5331957079404,2.91331917807891));
#14499=CARTESIAN_POINT('Ctrl Pts',(-204.964611334002,67.5214909567086,2.86034973847748));
#14500=CARTESIAN_POINT('Ctrl Pts',(-204.130631490227,67.5097862054768,2.80738029887604));
#14501=CARTESIAN_POINT('Ctrl Pts',(-203.303034210866,67.0433148529584,2.75441085927461));
#14502=CARTESIAN_POINT('Ctrl Pts',(-202.861185469285,66.3359047315519,2.70144141967317));
#14503=CARTESIAN_POINT('Ctrl Pts',(-202.614113147639,65.9403361928114,2.67182204727943));
#14504=CARTESIAN_POINT('Ctrl Pts',(-202.487656913234,65.4694307733786,2.64220267488568));
#14505=CARTESIAN_POINT('Ctrl Pts',(-202.486313063014,64.9991964084992,2.61258330249194));
#14506=CARTESIAN_POINT('Origin',(-205.,65.,9.));
#14507=CARTESIAN_POINT('',(-202.480291681284,64.9980775076607,1.61258330249194));
#14508=CARTESIAN_POINT('',(-202.479332509853,65.0014637523716,1.88741669750805));
#14509=CARTESIAN_POINT('',(-202.4825,65.,9.));
#14510=CARTESIAN_POINT('Ctrl Pts',(-202.479332509853,65.0014637523716,1.88741669750805));
#14511=CARTESIAN_POINT('Ctrl Pts',(-202.478740781633,65.0870774969918,1.892847702869));
#14512=CARTESIAN_POINT('Ctrl Pts',(-202.482723841763,65.1726355357681,1.89827870822995));
#14513=CARTESIAN_POINT('Ctrl Pts',(-202.491463117057,65.2577049615865,1.9037097135909));
#14514=CARTESIAN_POINT('Ctrl Pts',(-202.576698627627,66.0874002966744,1.95667915319234));
#14515=CARTESIAN_POINT('Ctrl Pts',(-203.114364546716,66.8706167924958,2.00964859279377));
#14516=CARTESIAN_POINT('Ctrl Pts',(-203.857997640336,67.2483325642607,2.06261803239521));
#14517=CARTESIAN_POINT('Ctrl Pts',(-204.601630733957,67.6260483360257,2.11558747199664));
#14518=CARTESIAN_POINT('Ctrl Pts',(-205.551231002108,67.5982633837343,2.16855691159808));
#14519=CARTESIAN_POINT('Ctrl Pts',(-206.271507076716,67.1777140868197,2.22152635119952));
#14520=CARTESIAN_POINT('Ctrl Pts',(-206.991783151323,66.7571647899052,2.27449579080095));
#14521=CARTESIAN_POINT('Ctrl Pts',(-207.482735032387,65.9438511483675,2.32746523040239));
#14522=CARTESIAN_POINT('Ctrl Pts',(-207.519313078463,65.1105916328361,2.38043467000382));
#14523=CARTESIAN_POINT('Ctrl Pts',(-207.555891124539,64.2773321173047,2.43340410960526));
#14524=CARTESIAN_POINT('Ctrl Pts',(-207.138095335629,63.4241267277794,2.48637354920669));
#14525=CARTESIAN_POINT('Ctrl Pts',(-206.457440987349,62.9420800261392,2.53934298880813));
#14526=CARTESIAN_POINT('Ctrl Pts',(-205.776786639069,62.460033324499,2.59231242840957));
#14527=CARTESIAN_POINT('Ctrl Pts',(-204.83327373142,62.3491453107438,2.645281868011));
#14528=CARTESIAN_POINT('Ctrl Pts',(-204.059403298444,62.660246440714,2.69825130761244));
#14529=CARTESIAN_POINT('Ctrl Pts',(-203.285532865468,62.9713475706841,2.75122074721387));
#14530=CARTESIAN_POINT('Ctrl Pts',(-202.681304907167,63.7044378443795,2.80419018681531));
#14531=CARTESIAN_POINT('Ctrl Pts',(-202.523694147865,64.5234727722695,2.85715962641674));
#14532=CARTESIAN_POINT('Ctrl Pts',(-202.493684139673,64.6794218014072,2.86724531678051));
#14533=CARTESIAN_POINT('Ctrl Pts',(-202.479865961982,64.8384867008611,2.87733100714428));
#14534=CARTESIAN_POINT('Ctrl Pts',(-202.481325106597,64.9978038277911,2.88741669750805));
#14535=CARTESIAN_POINT('Ctrl Pts',(-202.486313063014,64.9991964084992,2.61258330249194));
#14536=CARTESIAN_POINT('Ctrl Pts',(-202.485253655255,64.6284929419525,2.58923323528425));
#14537=CARTESIAN_POINT('Ctrl Pts',(-202.561948628095,64.2582065199014,2.56588316807656));
#14538=CARTESIAN_POINT('Ctrl Pts',(-202.718600866576,63.9255759514543,2.54253310086887));
#14539=CARTESIAN_POINT('Ctrl Pts',(-203.073965209252,63.1710061830575,2.48956366126743));
#14540=CARTESIAN_POINT('Ctrl Pts',(-203.840794098404,62.6102155365585,2.43659422166599));
#14541=CARTESIAN_POINT('Ctrl Pts',(-204.667577479677,62.5002671884707,2.38362478206456));
#14542=CARTESIAN_POINT('Ctrl Pts',(-205.49436086095,62.3903188403828,2.33065534246312));
#14543=CARTESIAN_POINT('Ctrl Pts',(-206.381098734343,62.7312127907059,2.27768590286169));
#14544=CARTESIAN_POINT('Ctrl Pts',(-206.92131536661,63.366685408653,2.22471646326025));
#14545=CARTESIAN_POINT('Ctrl Pts',(-207.461531998877,64.0021580266001,2.17174702365882));
#14546=CARTESIAN_POINT('Ctrl Pts',(-207.655227390017,64.932209312171,2.11877758405738));
#14547=CARTESIAN_POINT('Ctrl Pts',(-207.413612753018,65.7305084368602,2.06580814445595));
#14548=CARTESIAN_POINT('Ctrl Pts',(-207.171998116018,66.5288075615494,2.01283870485451));
#14549=CARTESIAN_POINT('Ctrl Pts',(-206.495073450879,67.1953545253569,1.95986926525307));
#14550=CARTESIAN_POINT('Ctrl Pts',(-205.693137039763,67.4246089886848,1.90689982565164));
#14551=CARTESIAN_POINT('Ctrl Pts',(-204.891200628647,67.6538634520127,1.8539303860502));
#14552=CARTESIAN_POINT('Ctrl Pts',(-203.964252471554,67.4458254148609,1.80096094644877));
#14553=CARTESIAN_POINT('Ctrl Pts',(-203.337200838176,66.8958561611357,1.74799150684733));
#14554=CARTESIAN_POINT('Ctrl Pts',(-202.802880568774,66.4272189641786,1.70285543872887));
#14555=CARTESIAN_POINT('Ctrl Pts',(-202.486315293188,65.710305364988,1.6577193706104));
#14556=CARTESIAN_POINT('Ctrl Pts',(-202.480291681284,64.9980775076607,1.61258330249194));
#14557=CARTESIAN_POINT('Origin',(-205.,65.,9.));
#14558=CARTESIAN_POINT('',(-202.480232429385,65.0018635099461,0.612583302491936));
#14559=CARTESIAN_POINT('',(-202.485823128102,65.0013539996937,0.887416697508052));
#14560=CARTESIAN_POINT('',(-202.4825,65.,9.));
#14561=CARTESIAN_POINT('',(-206.913465996665,66.6359872033749,0.));
#14562=CARTESIAN_POINT('Ctrl Pts',(-202.480232429385,65.0018635099461,0.612583302491936));
#14563=CARTESIAN_POINT('Ctrl Pts',(-202.486197578718,64.2874572406361,0.567297187132251));
#14564=CARTESIAN_POINT('Ctrl Pts',(-202.805075480509,63.5684921698319,0.522011071772566));
#14565=CARTESIAN_POINT('Ctrl Pts',(-203.34253206956,63.09963781157,0.476724956412881));
#14566=CARTESIAN_POINT('Ctrl Pts',(-203.971174515616,62.55123677486,0.423755516811446));
#14567=CARTESIAN_POINT('Ctrl Pts',(-204.898856375572,62.3450143916412,0.370786077210011));
#14568=CARTESIAN_POINT('Ctrl Pts',(-205.700051205779,62.576961421545,0.317816637608576));
#14569=CARTESIAN_POINT('Ctrl Pts',(-206.501246035986,62.8089084514488,0.264847198007142));
#14570=CARTESIAN_POINT('Ctrl Pts',(-207.175953836445,63.4790248944752,0.211877758405707));
#14571=CARTESIAN_POINT('Ctrl Pts',(-207.415129834976,64.2765861727607,0.158908318804272));
#14572=CARTESIAN_POINT('Ctrl Pts',(-207.654305833508,65.0741474510461,0.105938879202837));
#14573=CARTESIAN_POINT('Ctrl Pts',(-207.457950030113,65.9991535645905,0.0529694396014022));
#14574=CARTESIAN_POINT('Ctrl Pts',(-206.913465996665,66.635987203375,-3.2665312349373E-14));
#14575=CARTESIAN_POINT('',(-203.082854885701,66.6387832991579,-5.61437644333811E-15));
#14576=CARTESIAN_POINT('Origin',(-205.,65.,0.));
#14577=CARTESIAN_POINT('Ctrl Pts',(-203.082851846776,66.6387856087132,-3.81639164714898E-15));
#14578=CARTESIAN_POINT('Ctrl Pts',(-203.61482262847,67.259363488501,0.0519060689145044));
#14579=CARTESIAN_POINT('Ctrl Pts',(-204.477412313746,67.5988757717313,0.103812137829013));
#14580=CARTESIAN_POINT('Ctrl Pts',(-205.2894785266,67.5049507621395,0.155718206743521));
#14581=CARTESIAN_POINT('Ctrl Pts',(-206.118181087084,67.4091015632562,0.208687646344957));
#14582=CARTESIAN_POINT('Ctrl Pts',(-206.894268878324,66.8618739841832,0.261657085946393));
#14583=CARTESIAN_POINT('Ctrl Pts',(-207.26249802366,66.113605339536,0.314626525547829));
#14584=CARTESIAN_POINT('Ctrl Pts',(-207.630727168995,65.3653366948888,0.367595965149265));
#14585=CARTESIAN_POINT('Ctrl Pts',(-207.591097668426,64.4160269846675,0.420565404750701));
#14586=CARTESIAN_POINT('Ctrl Pts',(-207.161527535563,63.7010804522683,0.473534844352138));
#14587=CARTESIAN_POINT('Ctrl Pts',(-206.7319574027,62.9861339198691,0.526504283953574));
#14588=CARTESIAN_POINT('Ctrl Pts',(-205.912446637543,62.5055505652921,0.57947372355501));
#14589=CARTESIAN_POINT('Ctrl Pts',(-205.078774815322,62.4795076113936,0.632443163156446));
#14590=CARTESIAN_POINT('Ctrl Pts',(-204.245102993101,62.4534646574951,0.685412602757882));
#14591=CARTESIAN_POINT('Ctrl Pts',(-203.397270113817,62.881962104275,0.738382042359318));
#14592=CARTESIAN_POINT('Ctrl Pts',(-202.923859535018,63.5686371622738,0.791351481960754));
#14593=CARTESIAN_POINT('Ctrl Pts',(-202.637667536784,63.9837544321181,0.82337322047652));
#14594=CARTESIAN_POINT('Ctrl Pts',(-202.488311662699,64.4932251195213,0.855394958992286));
#14595=CARTESIAN_POINT('Ctrl Pts',(-202.485823128102,65.0013539996937,0.887416697508052));
#14596=CARTESIAN_POINT('Origin',(-205.,65.,-2.20842344717744));
#14597=CARTESIAN_POINT('',(-201.921327255612,65.0000400816385,16.2084234471775));
#14598=CARTESIAN_POINT('',(-201.931378751613,65.000780661492,16.2915765528226));
#14599=CARTESIAN_POINT('',(-201.9265,65.0000000000003,-2.20842344717744));
#14600=CARTESIAN_POINT('',(-205.793799282533,62.0307770462544,17.));
#14601=CARTESIAN_POINT('Ctrl Pts',(-201.931378751613,65.000780661492,16.2915765528226));
#14602=CARTESIAN_POINT('Ctrl Pts',(-201.930449348459,65.4711429475139,16.315839943476));
#14603=CARTESIAN_POINT('Ctrl Pts',(-202.253363219044,66.967050695802,16.3930727737308));
#14604=CARTESIAN_POINT('Ctrl Pts',(-204.58235401933,68.6092464457014,16.5232750435871));
#14605=CARTESIAN_POINT('Ctrl Pts',(-207.810233494003,67.3070985281123,16.6821833623914));
#14606=CARTESIAN_POINT('Ctrl Pts',(-208.456478816595,63.8847024923042,16.8410916811957));
#14607=CARTESIAN_POINT('Ctrl Pts',(-206.782006578242,62.2949667869872,16.9470305603986));
#14608=CARTESIAN_POINT('Ctrl Pts',(-205.793799282533,62.0307770462544,17.));
#14609=CARTESIAN_POINT('',(-204.206200717467,62.0307770462543,17.));
#14610=CARTESIAN_POINT('Origin',(-205.,65.,17.));
#14611=CARTESIAN_POINT('Ctrl Pts',(-201.921327255612,65.0000400816385,16.2084234471775));
#14612=CARTESIAN_POINT('Ctrl Pts',(-201.921327064386,65.0014822929036,16.2084984707981));
#14613=CARTESIAN_POINT('Ctrl Pts',(-201.921978896747,66.0211785478221,16.2615429340201));
#14614=CARTESIAN_POINT('Ctrl Pts',(-203.036142251593,68.0574739112173,16.3675568368436));
#14615=CARTESIAN_POINT('Ctrl Pts',(-206.506722984033,68.3070966859805,16.5264651556479));
#14616=CARTESIAN_POINT('Ctrl Pts',(-208.595801399242,65.5239883392264,16.6853734744522));
#14617=CARTESIAN_POINT('Ctrl Pts',(-207.396687980664,62.2840121808758,16.8432184225696));
#14618=CARTESIAN_POINT('Ctrl Pts',(-205.168807349915,61.7689270476826,16.9480939310855));
#14619=CARTESIAN_POINT('Ctrl Pts',(-204.204431285565,62.0254151804089,17.));
#14620=CARTESIAN_POINT('Origin',(-205.,65.,-2.20842344717744));
#14621=CARTESIAN_POINT('',(-201.92822561016,65.0026730836673,15.2084234471775));
#14622=CARTESIAN_POINT('',(-201.926883911247,64.9971795384332,15.2915765528226));
#14623=CARTESIAN_POINT('',(-201.9265,65.0000000000003,-2.20842344717744));
#14624=CARTESIAN_POINT('Ctrl Pts',(-201.926883911247,64.9971795384332,15.2915765528226));
#14625=CARTESIAN_POINT('Ctrl Pts',(-201.933858660338,65.7655048517695,15.3313566392007));
#14626=CARTESIAN_POINT('Ctrl Pts',(-202.614666302031,67.5679201912294,15.4241061651802));
#14627=CARTESIAN_POINT('Ctrl Pts',(-205.641600424982,68.5768349043511,15.5698251307612));
#14628=CARTESIAN_POINT('Ctrl Pts',(-208.354330159779,66.3978993048601,15.7287334495655));
#14629=CARTESIAN_POINT('Ctrl Pts',(-207.991779446085,62.9373177297799,15.8876417683699));
#14630=CARTESIAN_POINT('Ctrl Pts',(-204.886538861478,61.3679191982373,16.0465500871742));
#14631=CARTESIAN_POINT('Ctrl Pts',(-202.343324158449,62.8593293585014,16.1811950153251));
#14632=CARTESIAN_POINT('Ctrl Pts',(-201.932478329689,64.4442944309099,16.2628705038745));
#14633=CARTESIAN_POINT('Ctrl Pts',(-201.931378751613,65.000780661492,16.2915765528226));
#14634=CARTESIAN_POINT('Ctrl Pts',(-201.92822561016,65.0026730836673,15.2084234471775));
#14635=CARTESIAN_POINT('Ctrl Pts',(-201.925723697844,65.3041504713038,15.2240151665228));
#14636=CARTESIAN_POINT('Ctrl Pts',(-202.105046276089,66.6269190709931,15.2925763254696));
#14637=CARTESIAN_POINT('Ctrl Pts',(-204.001159776429,68.4939639011247,15.4141069240177));
#14638=CARTESIAN_POINT('Ctrl Pts',(-207.396164892643,67.7320116880119,15.5730152428221));
#14639=CARTESIAN_POINT('Ctrl Pts',(-208.594390772745,64.4653708967053,15.7319235616264));
#14640=CARTESIAN_POINT('Ctrl Pts',(-206.497323573879,61.6888943200732,15.8908318804307));
#14641=CARTESIAN_POINT('Ctrl Pts',(-203.029156356454,61.9478343561165,16.0496651756144));
#14642=CARTESIAN_POINT('Ctrl Pts',(-201.921462076895,63.9832280166276,16.1555290311966));
#14643=CARTESIAN_POINT('Ctrl Pts',(-201.921327255612,65.0000400816385,16.2084234471775));
#14644=CARTESIAN_POINT('Origin',(-205.,65.,-2.20842344717744));
#14645=CARTESIAN_POINT('',(-201.930818080783,64.9985876483626,14.2084234471775));
#14646=CARTESIAN_POINT('',(-201.921593038638,65.0008245362821,14.2915765528226));
#14647=CARTESIAN_POINT('',(-201.9265,65.0000000000003,-2.20842344717744));
#14648=CARTESIAN_POINT('Ctrl Pts',(-201.921593038638,65.0008245362821,14.2915765528226));
#14649=CARTESIAN_POINT('Ctrl Pts',(-201.921433171929,65.0455751138522,14.293903895324));
#14650=CARTESIAN_POINT('Ctrl Pts',(-201.94260765529,66.108677346403,14.3492006774268));
#14651=CARTESIAN_POINT('Ctrl Pts',(-203.167704085678,68.1381789685902,14.4574668991311));
#14652=CARTESIAN_POINT('Ctrl Pts',(-206.645674046841,68.2399430821141,14.6163752179354));
#14653=CARTESIAN_POINT('Ctrl Pts',(-208.614908869506,65.3713640210235,14.7752835367397));
#14654=CARTESIAN_POINT('Ctrl Pts',(-207.270034749662,62.1623216890685,14.934191855544));
#14655=CARTESIAN_POINT('Ctrl Pts',(-203.844019983521,61.5548329425339,15.0931001743483));
#14656=CARTESIAN_POINT('Ctrl Pts',(-202.070137533967,63.4672306219619,15.2122284067745));
#14657=CARTESIAN_POINT('Ctrl Pts',(-201.92457138662,64.7424361512098,15.2783871995992));
#14658=CARTESIAN_POINT('Ctrl Pts',(-201.926883911247,64.9971795384332,15.2915765528226));
#14659=CARTESIAN_POINT('Ctrl Pts',(-201.930818080783,64.9985876483626,14.2084234471775));
#14660=CARTESIAN_POINT('Ctrl Pts',(-201.93331444443,65.6013705544098,14.2395318622475));
#14661=CARTESIAN_POINT('Ctrl Pts',(-202.396541145728,67.2340750825248,14.323609716919));
#14662=CARTESIAN_POINT('Ctrl Pts',(-205.050996574037,68.6335759662945,14.4606570111919));
#14663=CARTESIAN_POINT('Ctrl Pts',(-208.082122938738,66.9250957063364,14.6195653299962));
#14664=CARTESIAN_POINT('Ctrl Pts',(-208.287593414598,63.4517090773303,14.7784736488005));
#14665=CARTESIAN_POINT('Ctrl Pts',(-205.479035047994,61.3977785533642,14.9373819676048));
#14666=CARTESIAN_POINT('Ctrl Pts',(-202.549962640807,62.5238193976047,15.0806985670638));
#14667=CARTESIAN_POINT('Ctrl Pts',(-201.934223395047,64.2799473079498,15.1710457269214));
#14668=CARTESIAN_POINT('Ctrl Pts',(-201.92822561016,65.0026730836673,15.2084234471775));
#14669=CARTESIAN_POINT('Origin',(-205.,65.,-2.20842344717744));
#14670=CARTESIAN_POINT('',(-201.923049085304,64.9979784157639,13.2084234471775));
#14671=CARTESIAN_POINT('',(-201.929343804705,65.0023490103727,13.2915765528226));
#14672=CARTESIAN_POINT('',(-201.9265,65.0000000000003,-2.20842344717744));
#14673=CARTESIAN_POINT('Ctrl Pts',(-201.929343804705,65.0023490103727,13.2915765528226));
#14674=CARTESIAN_POINT('Ctrl Pts',(-201.926890407685,65.3476938732414,13.3094205910487));
#14675=CARTESIAN_POINT('Ctrl Pts',(-202.140127765787,66.715242629014,13.3802340688762));
#14676=CARTESIAN_POINT('Ctrl Pts',(-204.150352559975,68.5332102455456,13.5040169863053));
#14677=CARTESIAN_POINT('Ctrl Pts',(-207.509958369796,67.627847859619,13.6629253051095));
#14678=CARTESIAN_POINT('Ctrl Pts',(-208.568462405179,64.313303932567,13.8218336239139));
#14679=CARTESIAN_POINT('Ctrl Pts',(-206.355439979715,61.6283152734234,13.9807419427182));
#14680=CARTESIAN_POINT('Ctrl Pts',(-202.950376540163,62.028501342373,14.1373229190211));
#14681=CARTESIAN_POINT('Ctrl Pts',(-201.925071678064,64.0270688070702,14.2409344557225));
#14682=CARTESIAN_POINT('Ctrl Pts',(-201.921593038638,65.0008245362821,14.2915765528226));
#14683=CARTESIAN_POINT('Ctrl Pts',(-201.923049085304,64.9979784157639,13.2084234471775));
#14684=CARTESIAN_POINT('Ctrl Pts',(-201.929872233322,65.8956158856996,13.2550485579722));
#14685=CARTESIAN_POINT('Ctrl Pts',(-202.81779490193,67.8247836690126,13.3546431083684));
#14686=CARTESIAN_POINT('Ctrl Pts',(-206.096501553054,68.4645576101642,13.5072070983661));
#14687=CARTESIAN_POINT('Ctrl Pts',(-208.506291890959,65.9546686696882,13.6661154171704));
#14688=CARTESIAN_POINT('Ctrl Pts',(-207.70155301198,62.5695501611123,13.8250237359747));
#14689=CARTESIAN_POINT('Ctrl Pts',(-204.420060527044,61.4126409040308,13.983932054779));
#14690=CARTESIAN_POINT('Ctrl Pts',(-202.208562006044,63.127226492007,14.1117319585132));
#14691=CARTESIAN_POINT('Ctrl Pts',(-201.929063794464,64.574989986234,14.1865624226461));
#14692=CARTESIAN_POINT('Ctrl Pts',(-201.930818080783,64.9985876483626,14.2084234471775));
#14693=CARTESIAN_POINT('Origin',(-205.,65.,-2.20842344717744));
#14694=CARTESIAN_POINT('',(-201.924541399743,65.0025681720917,12.2084234471775));
#14695=CARTESIAN_POINT('',(-201.930084889885,64.9980134264973,12.2915765528226));
#14696=CARTESIAN_POINT('',(-201.9265,65.0000000000003,-2.20842344717744));
#14697=CARTESIAN_POINT('Ctrl Pts',(-201.930084889885,64.9980134264973,12.2915765528226));
#14698=CARTESIAN_POINT('Ctrl Pts',(-201.933904699482,65.6440526195987,12.3249372867734));
#14699=CARTESIAN_POINT('Ctrl Pts',(-202.449144876912,67.3214312246058,12.4112674603257));
#14700=CARTESIAN_POINT('Ctrl Pts',(-205.205168523821,68.6281374401227,12.5505670734794));
#14701=CARTESIAN_POINT('Ctrl Pts',(-208.161051499856,66.7925481367497,12.7094753922837));
#14702=CARTESIAN_POINT('Ctrl Pts',(-208.218917791317,63.3135707366188,12.868383711088));
#14703=CARTESIAN_POINT('Ctrl Pts',(-205.325716228722,61.3806928361316,13.0272920298923));
#14704=CARTESIAN_POINT('Ctrl Pts',(-202.492315006707,62.6104022255164,13.1683563104705));
#14705=CARTESIAN_POINT('Ctrl Pts',(-201.934173235912,64.3225490252213,13.2564511514473));
#14706=CARTESIAN_POINT('Ctrl Pts',(-201.929343804705,65.0023490103727,13.2915765528226));
#14707=CARTESIAN_POINT('Ctrl Pts',(-201.924541399743,65.0025681720917,12.2084234471775));
#14708=CARTESIAN_POINT('Ctrl Pts',(-201.922957716369,65.1793797916405,12.2175958140955));
#14709=CARTESIAN_POINT('Ctrl Pts',(-202.017351358014,66.3755695754831,12.279737620615));
#14710=CARTESIAN_POINT('Ctrl Pts',(-203.586717704544,68.3478512877946,12.3948488667359));
#14711=CARTESIAN_POINT('Ctrl Pts',(-207.048871778231,68.0012663207677,12.5537571855402));
#14712=CARTESIAN_POINT('Ctrl Pts',(-208.632643105455,64.9031539354061,12.7126655043445));
#14713=CARTESIAN_POINT('Ctrl Pts',(-206.886047834894,61.8938289396112,12.8715738231488));
#14714=CARTESIAN_POINT('Ctrl Pts',(-203.410344989279,61.7322068549995,13.0304821419532));
#14715=CARTESIAN_POINT('Ctrl Pts',(-201.984214525019,63.7348656859119,13.1427653499627));
#14716=CARTESIAN_POINT('Ctrl Pts',(-201.922120652239,64.8758359229873,13.2020791183708));
#14717=CARTESIAN_POINT('Ctrl Pts',(-201.923049085304,64.9979784157639,13.2084234471775));
#14718=CARTESIAN_POINT('Origin',(-205.,65.,-2.20842344717744));
#14719=CARTESIAN_POINT('',(-201.93135070807,65.0005697538699,11.2084234471775));
#14720=CARTESIAN_POINT('',(-201.922104816116,64.9986005640695,11.2915765528226));
#14721=CARTESIAN_POINT('',(-201.9265,65.0000000000003,-2.20842344717744));
#14722=CARTESIAN_POINT('Ctrl Pts',(-201.922104816116,64.9986005640695,11.2915765528226));
#14723=CARTESIAN_POINT('Ctrl Pts',(-201.927430244541,65.9388404453587,11.3404539824981));
#14724=CARTESIAN_POINT('Ctrl Pts',(-202.890890835511,67.9074743145328,11.4423008517751));
#14725=CARTESIAN_POINT('Ctrl Pts',(-206.24255786536,68.4148975619695,11.5971171606536));
#14726=CARTESIAN_POINT('Ctrl Pts',(-208.54365094371,65.80499279292,11.7560254794579));
#14727=CARTESIAN_POINT('Ctrl Pts',(-207.595964443522,62.4570796285605,11.9149337982622));
#14728=CARTESIAN_POINT('Ctrl Pts',(-204.268326756069,61.4404874390394,12.0738421170665));
#14729=CARTESIAN_POINT('Ctrl Pts',(-202.169249555209,63.215545030581,12.1993897019199));
#14730=CARTESIAN_POINT('Ctrl Pts',(-201.92783968982,64.6182857983542,12.271967847172));
#14731=CARTESIAN_POINT('Ctrl Pts',(-201.930084889885,64.9980134264973,12.2915765528226));
#14732=CARTESIAN_POINT('Ctrl Pts',(-201.93135070807,65.0005697538699,11.2084234471775));
#14733=CARTESIAN_POINT('Ctrl Pts',(-201.930559327437,65.4791732627651,11.2331125098202));
#14734=CARTESIAN_POINT('Ctrl Pts',(-202.261422849189,66.9835666250466,11.3107710120644));
#14735=CARTESIAN_POINT('Ctrl Pts',(-204.61202606459,68.6131636161778,11.4413989539101));
#14736=CARTESIAN_POINT('Ctrl Pts',(-207.827214742755,67.2830531947759,11.6003072727144));
#14737=CARTESIAN_POINT('Ctrl Pts',(-208.450444543957,63.859865121617,11.7592155915187));
#14738=CARTESIAN_POINT('Ctrl Pts',(-205.910345352164,61.4819399619076,11.918123910323));
#14739=CARTESIAN_POINT('Ctrl Pts',(-202.730442829122,62.2804204494558,12.0678598622093));
#14740=CARTESIAN_POINT('Ctrl Pts',(-201.932103318763,64.1583115672449,12.1646263744941));
#14741=CARTESIAN_POINT('Ctrl Pts',(-201.924541399743,65.0025681720917,12.2084234471775));
#14742=CARTESIAN_POINT('Origin',(-205.,65.,-2.20842344717744));
#14743=CARTESIAN_POINT('',(-201.926636332893,64.997176114423,10.2084234471775));
#14744=CARTESIAN_POINT('',(-201.925849963783,65.0027879232472,10.2915765528225));
#14745=CARTESIAN_POINT('',(-201.9265,65.0000000000003,-2.20842344717744));
#14746=CARTESIAN_POINT('Ctrl Pts',(-201.925849963783,65.0027879232472,10.2915765528226));
#14747=CARTESIAN_POINT('Ctrl Pts',(-201.923807784004,65.2232580373303,10.3030012386214));
#14748=CARTESIAN_POINT('Ctrl Pts',(-202.046104360132,66.4636685168287,10.3673953640217));
#14749=CARTESIAN_POINT('Ctrl Pts',(-203.730082217424,68.4048177973288,10.4847589290234));
#14750=CARTESIAN_POINT('Ctrl Pts',(-207.174406712011,67.9116027988503,10.6436672478277));
#14751=CARTESIAN_POINT('Ctrl Pts',(-208.625259435921,64.7490628967685,10.802575566632));
#14752=CARTESIAN_POINT('Ctrl Pts',(-206.752514827754,61.816579326257,10.9614838854363));
#14753=CARTESIAN_POINT('Ctrl Pts',(-203.273084212998,61.8026202489985,11.1203922042406));
#14754=CARTESIAN_POINT('Ctrl Pts',(-201.9601129259,63.8226531889706,11.2304230933694));
#14755=CARTESIAN_POINT('Ctrl Pts',(-201.921658972173,64.9198838444615,11.2874845428967));
#14756=CARTESIAN_POINT('Ctrl Pts',(-201.922104816116,64.9986005640695,11.2915765528226));
#14757=CARTESIAN_POINT('Ctrl Pts',(-201.926636332893,64.997176114423,10.2084234471775));
#14758=CARTESIAN_POINT('Ctrl Pts',(-201.933743017009,65.7735626620793,10.248629205545));
#14759=CARTESIAN_POINT('Ctrl Pts',(-202.626478224698,67.5840970922976,10.3418044035139));
#14760=CARTESIAN_POINT('Ctrl Pts',(-205.670288190648,68.5715807191365,10.4879490410843));
#14761=CARTESIAN_POINT('Ctrl Pts',(-208.365419479959,66.3709218853546,10.6468573598885));
#14762=CARTESIAN_POINT('Ctrl Pts',(-207.975171804641,62.9134171895902,10.8057656786929));
#14763=CARTESIAN_POINT('Ctrl Pts',(-204.857319871709,61.3688682931048,10.9646739974972));
#14764=CARTESIAN_POINT('Ctrl Pts',(-202.334362743788,62.8760590219367,11.0988932536587));
#14765=CARTESIAN_POINT('Ctrl Pts',(-201.932257204317,64.45234773989,11.1801430702188));
#14766=CARTESIAN_POINT('Ctrl Pts',(-201.93135070807,65.0005697538699,11.2084234471775));
#14767=CARTESIAN_POINT('Origin',(-205.,65.,-2.20842344717744));
#14768=CARTESIAN_POINT('',(-201.921694845227,65.0009686859934,9.20842344717746));
#14769=CARTESIAN_POINT('',(-201.931440657504,64.9998541967196,9.29157655282255));
#14770=CARTESIAN_POINT('',(-201.9265,65.0000000000003,-2.20842344717744));
#14771=CARTESIAN_POINT('Ctrl Pts',(-201.931440657504,64.9998541967196,9.29157655282255));
#14772=CARTESIAN_POINT('Ctrl Pts',(-201.931661291496,65.5221576605085,9.31851793434613));
#14773=CARTESIAN_POINT('Ctrl Pts',(-202.306392258298,67.071658817483,9.39842875547113));
#14774=CARTESIAN_POINT('Ctrl Pts',(-204.765727205063,68.6263744518545,9.53130901619758));
#14775=CARTESIAN_POINT('Ctrl Pts',(-207.921565600238,67.1610020478975,9.69021733500189));
#14776=CARTESIAN_POINT('Ctrl Pts',(-208.398945306849,63.714447119501,9.84912565380619));
#14777=CARTESIAN_POINT('Ctrl Pts',(-205.76020994545,61.4464727035873,10.0080339726105));
#14778=CARTESIAN_POINT('Ctrl Pts',(-202.664341261103,62.3651666064549,10.1555176056159));
#14779=CARTESIAN_POINT('Ctrl Pts',(-201.933276151044,64.2010698916383,10.25003179902));
#14780=CARTESIAN_POINT('Ctrl Pts',(-201.925849963783,65.0027879232472,10.2915765528226));
#14781=CARTESIAN_POINT('Ctrl Pts',(-201.921694845227,65.0009686859933,9.20842344717746));
#14782=CARTESIAN_POINT('Ctrl Pts',(-201.921476487875,65.0539088334071,9.21117646166824));
#14783=CARTESIAN_POINT('Ctrl Pts',(-201.94672114028,66.12523254833,9.26689891576045));
#14784=CARTESIAN_POINT('Ctrl Pts',(-203.192942654321,68.1527795421275,9.37559080945409));
#14785=CARTESIAN_POINT('Ctrl Pts',(-206.671617316371,68.2266345686238,9.5344991282584));
#14786=CARTESIAN_POINT('Ctrl Pts',(-208.617771906093,65.3423470860332,9.69340744706271));
#14787=CARTESIAN_POINT('Ctrl Pts',(-207.247193647397,62.1441996213101,9.85231576586701));
#14788=CARTESIAN_POINT('Ctrl Pts',(-203.816413369187,61.5642180250794,10.0112240846713));
#14789=CARTESIAN_POINT('Ctrl Pts',(-202.064218289351,63.4839054024564,10.1299266451081));
#14790=CARTESIAN_POINT('Ctrl Pts',(-201.924380251815,64.7507051905809,10.1956597659435));
#14791=CARTESIAN_POINT('Ctrl Pts',(-201.926636332893,64.997176114423,10.2084234471775));
#14792=CARTESIAN_POINT('Origin',(-205.,65.,-2.20842344717744));
#14793=CARTESIAN_POINT('',(-201.92953466944,65.0022696572995,8.20842344717746));
#14794=CARTESIAN_POINT('',(-201.925313606426,64.9972772118362,8.29157655282255));
#14795=CARTESIAN_POINT('',(-201.9265,65.0000000000003,-2.20842344717744));
#14796=CARTESIAN_POINT('Ctrl Pts',(-201.925313606426,64.9972772118362,8.29157655282255));
#14797=CARTESIAN_POINT('Ctrl Pts',(-201.932861274056,65.8162531240691,8.33403463007084));
#14798=CARTESIAN_POINT('Ctrl Pts',(-202.690778828862,67.6692927338958,8.42946214692057));
#14799=CARTESIAN_POINT('Ctrl Pts',(-205.821270877028,68.5399137777715,8.57785910337175));
#14800=CARTESIAN_POINT('Ctrl Pts',(-208.420572279286,66.2268499051207,8.73676742217605));
#14801=CARTESIAN_POINT('Ctrl Pts',(-207.883931246923,62.7890237517031,8.89567574098036));
#14802=CARTESIAN_POINT('Ctrl Pts',(-204.703334280485,61.3781959110996,9.05458405978466));
#14803=CARTESIAN_POINT('Ctrl Pts',(-202.287845274185,62.9640429293115,9.1865509970654));
#14804=CARTESIAN_POINT('Ctrl Pts',(-201.931227503092,64.4952570260857,9.26554849474469));
#14805=CARTESIAN_POINT('Ctrl Pts',(-201.931440657504,64.9998541967196,9.29157655282255));
#14806=CARTESIAN_POINT('Ctrl Pts',(-201.92953466944,65.0022696572995,8.20842344717746));
#14807=CARTESIAN_POINT('Ctrl Pts',(-201.927117444002,65.3559080588384,8.22669315739295));
#14808=CARTESIAN_POINT('Ctrl Pts',(-202.147019533078,66.7319379190628,8.29793230720988));
#14809=CARTESIAN_POINT('Ctrl Pts',(-204.178729132788,68.5399137354599,8.42214089662826));
#14810=CARTESIAN_POINT('Ctrl Pts',(-207.530962455862,67.6076242326776,8.58104921543256));
#14811=CARTESIAN_POINT('Ctrl Pts',(-208.562837687446,64.2846939782535,8.73995753423686));
#14812=CARTESIAN_POINT('Ctrl Pts',(-206.328343148279,61.6175482897389,8.89886585304117));
#14813=CARTESIAN_POINT('Ctrl Pts',(-202.935848069069,62.0438803005006,9.0550211573547));
#14814=CARTESIAN_POINT('Ctrl Pts',(-201.925677797602,64.0353126907724,9.1582070220668));
#14815=CARTESIAN_POINT('Ctrl Pts',(-201.921694845227,65.0009686859933,9.20842344717746));
#14816=CARTESIAN_POINT('Origin',(-205.,65.,-2.20842344717744));
#14817=CARTESIAN_POINT('',(-201.929918596978,64.9979181762371,7.20842344717746));
#14818=CARTESIAN_POINT('',(-201.922453672097,65.0016690942922,7.29157655282255));
#14819=CARTESIAN_POINT('',(-201.9265,65.0000000000003,-2.20842344717744));
#14820=CARTESIAN_POINT('Ctrl Pts',(-201.922453672097,65.0016690942922,7.29157655282255));
#14821=CARTESIAN_POINT('Ctrl Pts',(-201.921823212738,65.0979839665099,7.29658188619413));
#14822=CARTESIAN_POINT('Ctrl Pts',(-201.969645797573,66.2129262637451,7.35455665916715));
#14823=CARTESIAN_POINT('Ctrl Pts',(-203.328382663649,68.2266346071907,7.4655008717416));
#14824=CARTESIAN_POINT('Ctrl Pts',(-206.807057367278,68.1527795798118,7.62440919054589));
#14825=CARTESIAN_POINT('Ctrl Pts',(-208.629042073693,65.1884914716269,7.78331750935022));
#14826=CARTESIAN_POINT('Ctrl Pts',(-207.123961567999,62.0513964889848,7.94222582815451));
#14827=CARTESIAN_POINT('Ctrl Pts',(-203.671656835844,61.6175482493094,8.10113414695882));
#14828=CARTESIAN_POINT('Ctrl Pts',(-202.03418792352,63.5720699870132,8.21758438851483));
#14829=CARTESIAN_POINT('Ctrl Pts',(-201.923445027477,64.7945230333643,8.28106519046941));
#14830=CARTESIAN_POINT('Ctrl Pts',(-201.925313606426,64.9972772118362,8.29157655282255));
#14831=CARTESIAN_POINT('Ctrl Pts',(-201.929918596978,64.9979181762371,7.20842344717746));
#14832=CARTESIAN_POINT('Ctrl Pts',(-201.93398631635,65.6521116579694,7.24220985311768));
#14833=CARTESIAN_POINT('Ctrl Pts',(-202.459399722692,67.3378982854403,7.32896569865932));
#14834=CARTESIAN_POINT('Ctrl Pts',(-205.234272792136,68.6263744085096,7.46869098380242));
#14835=CARTESIAN_POINT('Ctrl Pts',(-208.175332472178,66.7671272684671,7.62759930260672));
#14836=CARTESIAN_POINT('Ctrl Pts',(-208.205282831762,63.2877975995101,7.78650762141103));
#14837=CARTESIAN_POINT('Ctrl Pts',(-205.29666571597,61.3781959543899,7.94541594021533));
#14838=CARTESIAN_POINT('Ctrl Pts',(-202.481742432778,62.6268207185444,8.08605454880415));
#14839=CARTESIAN_POINT('Ctrl Pts',(-201.934125714812,64.3306029100366,8.17372371779152));
#14840=CARTESIAN_POINT('Ctrl Pts',(-201.92953466944,65.0022696572995,8.20842344717746));
#14841=CARTESIAN_POINT('Origin',(-205.,65.,-2.20842344717744));
#14842=CARTESIAN_POINT('',(-201.921960580212,64.9987333336508,6.20842344717746));
#14843=CARTESIAN_POINT('',(-201.930412916854,65.0017670725165,6.29157655282255));
#14844=CARTESIAN_POINT('',(-201.9265,65.0000000000003,-2.20842344717744));
#14845=CARTESIAN_POINT('Ctrl Pts',(-201.930412916854,65.0017670725165,6.29157655282255));
#14846=CARTESIAN_POINT('Ctrl Pts',(-201.928336333622,65.3992879077885,6.31209858191885));
#14847=CARTESIAN_POINT('Ctrl Pts',(-202.184898002603,66.8202733387973,6.38559005061658));
#14848=CARTESIAN_POINT('Ctrl Pts',(-204.32971180134,68.5715807618264,6.51205095891576));
#14849=CARTESIAN_POINT('Ctrl Pts',(-207.639355851724,67.4978542982895,6.67095927772006));
#14850=CARTESIAN_POINT('Ctrl Pts',(-208.529267956781,64.1341229320817,6.82986759652437));
#14851=CARTESIAN_POINT('Ctrl Pts',(-206.18358664496,61.5642179840126,6.98877591532868));
#14852=CARTESIAN_POINT('Ctrl Pts',(-202.860869889385,62.1259311837648,7.1426789007614));
#14853=CARTESIAN_POINT('Ctrl Pts',(-201.92849511178,64.0787222254988,7.2436124465927));
#14854=CARTESIAN_POINT('Ctrl Pts',(-201.922453672097,65.0016690942922,7.29157655282255));
#14855=CARTESIAN_POINT('Ctrl Pts',(-201.921960580212,64.9987333336508,6.20842344717746));
#14856=CARTESIAN_POINT('Ctrl Pts',(-201.926898162024,65.9470439039035,6.2577265488424));
#14857=CARTESIAN_POINT('Ctrl Pts',(-202.905060880587,67.9229822365129,6.35999909010877));
#14858=CARTESIAN_POINT('Ctrl Pts',(-206.269917767397,68.4048177566322,6.51524107097658));
#14859=CARTESIAN_POINT('Ctrl Pts',(-208.549995805274,65.7765338848791,6.67414938978088));
#14860=CARTESIAN_POINT('Ctrl Pts',(-207.575477366445,62.4363324266277,6.83305770858519));
#14861=CARTESIAN_POINT('Ctrl Pts',(-204.239790063637,61.4464727460615,6.99196602738949));
#14862=CARTESIAN_POINT('Ctrl Pts',(-202.162091334594,63.2322401369024,7.11708794025358));
#14863=CARTESIAN_POINT('Ctrl Pts',(-201.927609052785,64.6264843041873,7.18924041351624));
#14864=CARTESIAN_POINT('Ctrl Pts',(-201.929918596978,64.9979181762371,7.20842344717746));
#14865=CARTESIAN_POINT('Origin',(-205.,65.,-2.20842344717744));
#14866=CARTESIAN_POINT('',(-201.926100634672,65.0028070195242,5.20842344717746));
#14867=CARTESIAN_POINT('',(-201.928910969323,64.9974995382691,5.29157655282255));
#14868=CARTESIAN_POINT('',(-201.9265,65.0000000000003,-2.20842344717744));
#14869=CARTESIAN_POINT('Ctrl Pts',(-201.928910969323,64.9974995382691,5.29157655282255));
#14870=CARTESIAN_POINT('Ctrl Pts',(-201.934235720436,65.6947278648159,5.32761527764357));
#14871=CARTESIAN_POINT('Ctrl Pts',(-202.515344024246,67.4247683985249,5.41662344206603));
#14872=CARTESIAN_POINT('Ctrl Pts',(-205.387973940047,68.613163659365,5.55860104608992));
#14873=CARTESIAN_POINT('Ctrl Pts',(-208.247472484712,66.6307660373427,5.71750936489423));
#14874=CARTESIAN_POINT('Ctrl Pts',(-208.129724551721,63.1533003390197,5.87641768369853));
#14875=CARTESIAN_POINT('Ctrl Pts',(-205.142680129997,61.368868249703,6.03532600250284));
#14876=CARTESIAN_POINT('Ctrl Pts',(-202.427479508272,62.7139482003332,6.17371229221085));
#14877=CARTESIAN_POINT('Ctrl Pts',(-201.933696205667,64.3732462929244,6.25912914231742));
#14878=CARTESIAN_POINT('Ctrl Pts',(-201.930412916854,65.0017670725165,6.29157655282255));
#14879=CARTESIAN_POINT('Ctrl Pts',(-201.926100634672,65.0028070195242,5.20842344717746));
#14880=CARTESIAN_POINT('Ctrl Pts',(-201.923984761182,65.2315394103251,5.22027380496568));
#14881=CARTESIAN_POINT('Ctrl Pts',(-202.051779433128,66.4803311623585,5.28509360235534));
#14882=CARTESIAN_POINT('Ctrl Pts',(-203.757442149492,68.4148975211522,5.40288283934643));
#14883=CARTESIAN_POINT('Ctrl Pts',(-207.197698349872,67.894062379217,5.56179115815073));
#14884=CARTESIAN_POINT('Ctrl Pts',(-208.623129266309,64.7199831943528,5.72069947695504));
#14885=CARTESIAN_POINT('Ctrl Pts',(-206.726915766361,61.8026202872159,5.87960779575935));
#14886=CARTESIAN_POINT('Ctrl Pts',(-203.247485193193,61.8165793643074,6.03851611456365));
#14887=CARTESIAN_POINT('Ctrl Pts',(-201.955780778247,63.8392267441314,6.14812133170303));
#14888=CARTESIAN_POINT('Ctrl Pts',(-201.921593405675,64.9282138956866,6.20475710924096));
#14889=CARTESIAN_POINT('Ctrl Pts',(-201.921960580212,64.9987333336508,6.20842344717746));
#14890=CARTESIAN_POINT('Origin',(-205.,65.,-2.20842344717744));
#14891=CARTESIAN_POINT('',(-201.931423654547,64.9997186192924,4.20842344717746));
#14892=CARTESIAN_POINT('',(-201.921426709108,64.9994934768783,4.29157655282255));
#14893=CARTESIAN_POINT('',(-201.9265,65.0000000000003,-2.20842344717744));
#14894=CARTESIAN_POINT('Ctrl Pts',(-201.921426709108,64.9994934768783,4.29157655282255));
#14895=CARTESIAN_POINT('Ctrl Pts',(-201.923689577646,65.9906673436395,4.34313197336829));
#14896=CARTESIAN_POINT('Ctrl Pts',(-202.981935595717,68.0043503849495,4.44765683351547));
#14897=CARTESIAN_POINT('Ctrl Pts',(-206.413282312349,68.3478513278105,4.60515113326408));
#14898=CARTESIAN_POINT('Ctrl Pts',(-208.579754999423,65.6251636198798,4.76405945206838));
#14899=CARTESIAN_POINT('Ctrl Pts',(-207.464348313206,62.3293328925706,4.92296777087269));
#14900=CARTESIAN_POINT('Ctrl Pts',(-204.089654636955,61.4819399198572,5.081876089677));
#14901=CARTESIAN_POINT('Ctrl Pts',(-202.125623034005,63.3205768432535,5.20474568366028));
#14902=CARTESIAN_POINT('Ctrl Pts',(-201.926409442345,64.6699470515422,5.27464583804213));
#14903=CARTESIAN_POINT('Ctrl Pts',(-201.928910969323,64.9974995382691,5.29157655282255));
#14904=CARTESIAN_POINT('Ctrl Pts',(-201.931423654547,64.9997186192924,4.20842344717746));
#14905=CARTESIAN_POINT('Ctrl Pts',(-201.931856309214,65.5302670894482,4.2357905006904));
#14906=CARTESIAN_POINT('Ctrl Pts',(-202.315183242628,67.0882876073577,4.31612699380478));
#14907=CARTESIAN_POINT('Ctrl Pts',(-204.794831478631,68.6281373967567,4.44943292652058));
#14908=CARTESIAN_POINT('Ctrl Pts',(-207.938810626636,67.1374908637484,4.60834124532489));
#14909=CARTESIAN_POINT('Ctrl Pts',(-208.388521038603,63.6872165971666,4.7672495641292));
#14910=CARTESIAN_POINT('Ctrl Pts',(-205.731673235186,61.4404874815853,4.92615788293351));
#14911=CARTESIAN_POINT('Ctrl Pts',(-202.652189346928,62.3812687692724,5.07321584394959));
#14912=CARTESIAN_POINT('Ctrl Pts',(-201.933442419344,64.209137658754,5.16730436536424));
#14913=CARTESIAN_POINT('Ctrl Pts',(-201.926100634672,65.0028070195242,5.20842344717746));
#14914=CARTESIAN_POINT('Origin',(-205.,65.,-2.20842344717744));
#14915=CARTESIAN_POINT('',(-201.925065626664,64.9973187943263,3.20842344717745));
#14916=CARTESIAN_POINT('',(-201.927406901239,65.0027899110459,3.29157655282255));
#14917=CARTESIAN_POINT('',(-201.9265,65.0000000000003,-2.20842344717744));
#14918=CARTESIAN_POINT('Ctrl Pts',(-201.927406901239,65.0027899110459,3.29157655282255));
#14919=CARTESIAN_POINT('Ctrl Pts',(-201.924995843745,65.2752913043072,3.30567922949157));
#14920=CARTESIAN_POINT('Ctrl Pts',(-202.083109248922,66.5685525880974,3.37275134576203));
#14921=CARTESIAN_POINT('Ctrl Pts',(-203.90349843384,68.4645576515751,3.49279290163393));
#14922=CARTESIAN_POINT('Ctrl Pts',(-207.318549180862,67.7981788906371,3.65170122043823));
#14923=CARTESIAN_POINT('Ctrl Pts',(-208.607979952898,64.5664609969902,3.81060953924254));
#14924=CARTESIAN_POINT('Ctrl Pts',(-206.589655029722,61.7322068159406,3.96951785804685));
#14925=CARTESIAN_POINT('Ctrl Pts',(-203.113952142563,61.893828902484,4.12842617685116));
#14926=CARTESIAN_POINT('Ctrl Pts',(-201.934013495981,63.9268235650214,4.23577907510972));
#14927=CARTESIAN_POINT('Ctrl Pts',(-201.921364645038,64.9723083871191,4.29016253376685));
#14928=CARTESIAN_POINT('Ctrl Pts',(-201.921426709108,64.9994934768783,4.29157655282255));
#14929=CARTESIAN_POINT('Ctrl Pts',(-201.925065626664,64.9973187943263,3.20842344717745));
#14930=CARTESIAN_POINT('Ctrl Pts',(-201.932640043333,65.8243336692917,3.25130719641511));
#14931=CARTESIAN_POINT('Ctrl Pts',(-202.703271173878,67.6853099211375,3.34716038525421));
#14932=CARTESIAN_POINT('Ctrl Pts',(-205.849647429869,68.5332102033146,3.49598301369475));
#14933=CARTESIAN_POINT('Ctrl Pts',(-208.430305934935,66.1993649512308,3.65489133249905));
#14934=CARTESIAN_POINT('Ctrl Pts',(-207.866098297326,62.7659553182491,3.81379965130336));
#14935=CARTESIAN_POINT('Ctrl Pts',(-204.674283775171,61.380692879392,3.97270797010767));
#14936=CARTESIAN_POINT('Ctrl Pts',(-202.279346917231,62.9806921969728,4.10424923539903));
#14937=CARTESIAN_POINT('Ctrl Pts',(-201.931018898082,64.5033806863407,4.18282106108896));
#14938=CARTESIAN_POINT('Ctrl Pts',(-201.931423654547,64.9997186192924,4.20842344717746));
#14939=CARTESIAN_POINT('Origin',(-205.,65.,-2.20842344717744));
#14940=CARTESIAN_POINT('',(-201.922632956914,65.0017870279701,2.20842344717745));
#14941=CARTESIAN_POINT('',(-201.931155193317,64.9990189320844,2.29157655282255));
#14942=CARTESIAN_POINT('',(-201.9265,65.0000000000003,-2.20842344717744));
#14943=CARTESIAN_POINT('Ctrl Pts',(-201.931155193316,64.9990189320844,2.29157655282255));
#14944=CARTESIAN_POINT('Ctrl Pts',(-201.932795838262,65.5731064476581,2.32119592521629));
#14945=CARTESIAN_POINT('Ctrl Pts',(-202.363272241673,67.1761406694018,2.40378473721147));
#14946=CARTESIAN_POINT('Ctrl Pts',(-204.949003425354,68.6335760097311,2.53934298880809));
#14947=CARTESIAN_POINT('Ctrl Pts',(-208.026882902896,67.010834485032,2.6982513076124));
#14948=CARTESIAN_POINT('Ctrl Pts',(-208.329749972245,63.5445823456684,2.8571596264167));
#14949=CARTESIAN_POINT('Ctrl Pts',(-205.579939479888,61.4126408611514,3.01606794522101));
#14950=CARTESIAN_POINT('Ctrl Pts',(-202.589670400847,62.4668776130536,3.16087358735629));
#14951=CARTESIAN_POINT('Ctrl Pts',(-201.93405173911,64.2517802056398,3.25270978989014));
#14952=CARTESIAN_POINT('Ctrl Pts',(-201.927406901239,65.0027899110459,3.29157655282255));
#14953=CARTESIAN_POINT('Ctrl Pts',(-201.922632956914,65.0017870279701,2.20842344717745));
#14954=CARTESIAN_POINT('Ctrl Pts',(-201.921910543138,65.106308912415,2.2138544525384));
#14955=CARTESIAN_POINT('Ctrl Pts',(-201.974200288337,66.229517676892,2.27225489750078));
#14956=CARTESIAN_POINT('Ctrl Pts',(-203.354325972851,68.2399430433535,2.3836247820646));
#14957=CARTESIAN_POINT('Ctrl Pts',(-206.83229589241,68.1381789310981,2.54253310086891));
#14958=CARTESIAN_POINT('Ctrl Pts',(-208.630437627999,65.1593672402151,2.70144141967321));
#14959=CARTESIAN_POINT('Ctrl Pts',(-207.100234620393,62.0344495464248,2.86034973847752));
#14960=CARTESIAN_POINT('Ctrl Pts',(-203.644560036488,61.6283153137219,3.01925805728183));
#14961=CARTESIAN_POINT('Ctrl Pts',(-202.028754311406,63.5887202320378,3.13528262684847));
#14962=CARTESIAN_POINT('Ctrl Pts',(-201.923284224092,64.8028158391646,3.19833775681368));
#14963=CARTESIAN_POINT('Ctrl Pts',(-201.925065626664,64.9973187943263,3.20842344717745));
#14964=CARTESIAN_POINT('Origin',(-205.,65.,-2.20842344717744));
#14965=CARTESIAN_POINT('',(-201.930557054308,65.0016530359719,1.20842344717746));
#14966=CARTESIAN_POINT('',(-201.923803965215,64.9976529174956,1.29157655282255));
#14967=CARTESIAN_POINT('',(-201.9265,65.0000000000003,-2.20842344717744));
#14968=CARTESIAN_POINT('Ctrl Pts',(-201.923803965215,64.9976529174956,1.29157655282255));
#14969=CARTESIAN_POINT('Ctrl Pts',(-201.931157916033,65.8671791615852,1.33671262094101));
#14970=CARTESIAN_POINT('Ctrl Pts',(-202.771191556777,67.7695720873782,1.43481812866091));
#14971=CARTESIAN_POINT('Ctrl Pts',(-205.998840235539,68.4939639431765,1.58589307598225));
#14972=CARTESIAN_POINT('Ctrl Pts',(-208.478118835308,66.0526943186335,1.74480139478656));
#14973=CARTESIAN_POINT('Ctrl Pts',(-207.768697443447,62.6463237610936,1.90370971359086));
#14974=CARTESIAN_POINT('Ctrl Pts',(-204.520964946279,61.3977785102674,2.06261803239517));
#14975=CARTESIAN_POINT('Ctrl Pts',(-202.235901714706,63.0688711165209,2.19190697880573));
#14976=CARTESIAN_POINT('Ctrl Pts',(-201.929861811092,64.5464441140382,2.26822648561486));
#14977=CARTESIAN_POINT('Ctrl Pts',(-201.931155193316,64.9990189320844,2.29157655282255));
#14978=CARTESIAN_POINT('Ctrl Pts',(-201.930557054308,65.0016530359719,1.20842344717746));
#14979=CARTESIAN_POINT('Ctrl Pts',(-201.928569592085,65.4074689546327,1.22937114826312));
#14980=CARTESIAN_POINT('Ctrl Pts',(-202.192314144726,66.836978287187,1.30328828895022));
#14981=CARTESIAN_POINT('Ctrl Pts',(-204.358399583502,68.5768348597731,1.43017486923876));
#14982=CARTESIAN_POINT('Ctrl Pts',(-207.659308320785,67.4766010095058,1.58908318804307));
#14983=CARTESIAN_POINT('Ctrl Pts',(-208.522208970686,64.1058310992964,1.74799150684737));
#14984=CARTESIAN_POINT('Ctrl Pts',(-206.155980002522,61.5548329839681,1.90689982565168));
#14985=CARTESIAN_POINT('Ctrl Pts',(-202.847056091155,62.1415595964765,2.06037713909504));
#14986=CARTESIAN_POINT('Ctrl Pts',(-201.928956357011,64.0868907242207,2.16088501293697));
#14987=CARTESIAN_POINT('Ctrl Pts',(-201.922632956914,65.0017870279701,2.20842344717745));
#14988=CARTESIAN_POINT('Origin',(-205.,65.,-2.20842344717744));
#14989=CARTESIAN_POINT('',(-201.929611540575,64.9968423971894,0.208423447177456));
#14990=CARTESIAN_POINT('',(-201.923731627295,65.0022750736125,0.291576552822547));
#14991=CARTESIAN_POINT('',(-201.9265,65.0000000000003,-2.20842344717744));
#14992=CARTESIAN_POINT('',(-204.206200717467,62.0307770462543,0.));
#14993=CARTESIAN_POINT('Ctrl Pts',(-204.206200717467,62.0307770462543,-5.55111512312578E-16));
#14994=CARTESIAN_POINT('Ctrl Pts',(-203.217993421758,62.2949667869871,0.052969439601435));
#14995=CARTESIAN_POINT('Ctrl Pts',(-202.119878197412,63.3375116748876,0.12244392199392));
#14996=CARTESIAN_POINT('Ctrl Pts',(-201.92719200432,64.6776063340067,0.191918404386406));
#14997=CARTESIAN_POINT('Ctrl Pts',(-201.929611540575,64.9968423971894,0.208423447177456));
#14998=CARTESIAN_POINT('',(-205.795567263823,62.0254195780229,4.05472878785602E-15));
#14999=CARTESIAN_POINT('Origin',(-205.,65.,0.));
#15000=CARTESIAN_POINT('Ctrl Pts',(-205.795568724168,62.0254151527766,-1.60732972070976E-16));
#15001=CARTESIAN_POINT('Ctrl Pts',(-204.831192689899,61.7689270501568,0.051906068914496));
#15002=CARTESIAN_POINT('Ctrl Pts',(-202.766529559188,62.2462762443893,0.149098253188679));
#15003=CARTESIAN_POINT('Ctrl Pts',(-201.931014203849,64.1300893064926,0.246290437462861));
#15004=CARTESIAN_POINT('Ctrl Pts',(-201.923731627295,65.0022750736125,0.291576552822547));
#15005=CARTESIAN_POINT('Origin',(-205.,-65.,9.));
#15006=CARTESIAN_POINT('',(-202.486496099891,-64.9993605807166,16.612583302492));
#15007=CARTESIAN_POINT('',(-202.484570781149,-65.0037022516384,16.887416697508));
#15008=CARTESIAN_POINT('',(-202.4825,-65.,9.));
#15009=CARTESIAN_POINT('',(-203.086534003335,-63.3640127966251,17.));
#15010=CARTESIAN_POINT('Ctrl Pts',(-202.484570781149,-65.0037022516384,
16.887416697508));
#15011=CARTESIAN_POINT('Ctrl Pts',(-202.489763089819,-64.4110264481633,
16.9249444650053));
#15012=CARTESIAN_POINT('Ctrl Pts',(-202.700778171916,-63.8151964396956,
16.9624722325027));
#15013=CARTESIAN_POINT('Ctrl Pts',(-203.086534003335,-63.3640127966251,
17.));
#15014=CARTESIAN_POINT('',(-202.4825,-65.,17.));
#15015=CARTESIAN_POINT('Origin',(-205.,-65.,17.));
#15016=CARTESIAN_POINT('',(-202.4825,-65.,18.));
#15017=CARTESIAN_POINT('',(-202.4825,-65.,9.));
#15018=CARTESIAN_POINT('Origin',(-205.,-65.,18.));
#15019=CARTESIAN_POINT('',(-206.917145184219,-63.36121664977,17.));
#15020=CARTESIAN_POINT('Origin',(-205.,-65.,17.));
#15021=CARTESIAN_POINT('Ctrl Pts',(-206.917148223239,-63.3612143401441,
17.));
#15022=CARTESIAN_POINT('Ctrl Pts',(-206.385177464426,-62.7406365841492,
16.9480939310855));
#15023=CARTESIAN_POINT('Ctrl Pts',(-205.522587726062,-62.4011240872398,
16.896187862171));
#15024=CARTESIAN_POINT('Ctrl Pts',(-204.710521467437,-62.4950490586621,
16.8442817932565));
#15025=CARTESIAN_POINT('Ctrl Pts',(-203.881818860243,-62.5908982185939,
16.7913123536551));
#15026=CARTESIAN_POINT('Ctrl Pts',(-203.105731029912,-63.1381259414902,
16.7383429140536));
#15027=CARTESIAN_POINT('Ctrl Pts',(-202.737501870931,-63.8863946460724,
16.6853734744522));
#15028=CARTESIAN_POINT('Ctrl Pts',(-202.568829368417,-64.2291495634286,
16.6611100837988));
#15029=CARTESIAN_POINT('Ctrl Pts',(-202.485734824973,-64.614087418431,16.6368466931454));
#15030=CARTESIAN_POINT('Ctrl Pts',(-202.486496099891,-64.9993605807166,
16.612583302492));
#15031=CARTESIAN_POINT('Origin',(-205.,-65.,9.));
#15032=CARTESIAN_POINT('',(-202.48281438265,-65.0023102366302,15.612583302492));
#15033=CARTESIAN_POINT('',(-202.478262929558,-64.9999671733494,15.887416697508));
#15034=CARTESIAN_POINT('',(-202.4825,-65.,9.));
#15035=CARTESIAN_POINT('Ctrl Pts',(-202.478262929558,-64.9999671733494,
15.887416697508));
#15036=CARTESIAN_POINT('Ctrl Pts',(-202.478152183127,-64.1647350270545,
15.9404611607301));
#15037=CARTESIAN_POINT('Ctrl Pts',(-202.934430543867,-63.3296386377248,
15.9935056239521));
#15038=CARTESIAN_POINT('Ctrl Pts',(-203.637206926075,-62.8782359116843,
16.0465500871742));
#15039=CARTESIAN_POINT('Ctrl Pts',(-204.338989334068,-62.4274716286557,
16.0995195267756));
#15040=CARTESIAN_POINT('Ctrl Pts',(-205.286572151919,-62.3593164180464,
16.152488966377));
#15041=CARTESIAN_POINT('Ctrl Pts',(-206.045557144883,-62.7051788961069,
16.2054584059785));
#15042=CARTESIAN_POINT('Ctrl Pts',(-206.804542137847,-63.0510413741674,
16.2584278455799));
#15043=CARTESIAN_POINT('Ctrl Pts',(-207.374929305926,-63.8109215408977,
16.3113972851813));
#15044=CARTESIAN_POINT('Ctrl Pts',(-207.495321385823,-64.636151503456,16.3643667247828));
#15045=CARTESIAN_POINT('Ctrl Pts',(-207.61571346572,-65.4613814660144,16.4173361643842));
#15046=CARTESIAN_POINT('Ctrl Pts',(-207.286110457436,-66.3519612244009,
16.4703056039856));
#15047=CARTESIAN_POINT('Ctrl Pts',(-206.657467982026,-66.9003622583766,
16.5232750435871));
#15048=CARTESIAN_POINT('Ctrl Pts',(-206.028825506615,-67.4487632923523,
16.5762444831885));
#15049=CARTESIAN_POINT('Ctrl Pts',(-205.101143564078,-67.6549856019172,
16.6292139227899));
#15050=CARTESIAN_POINT('Ctrl Pts',(-204.299948783103,-67.4230386209089,
16.6821833623914));
#15051=CARTESIAN_POINT('Ctrl Pts',(-203.498754002127,-67.1910916399006,
16.7351528019928));
#15052=CARTESIAN_POINT('Ctrl Pts',(-202.824046382713,-66.520975368319,16.7881222415943));
#15053=CARTESIAN_POINT('Ctrl Pts',(-202.584870374653,-65.7234140671963,
16.8410916811957));
#15054=CARTESIAN_POINT('Ctrl Pts',(-202.515145689638,-65.4909086794192,
16.8565333532998));
#15055=CARTESIAN_POINT('Ctrl Pts',(-202.482434285074,-65.2475724851116,
16.8719750254039));
#15056=CARTESIAN_POINT('Ctrl Pts',(-202.484570781149,-65.0037022516384,
16.887416697508));
#15057=CARTESIAN_POINT('Ctrl Pts',(-202.486496099891,-64.9993605807166,
16.612583302492));
#15058=CARTESIAN_POINT('Ctrl Pts',(-202.487396765235,-65.4551777586583,
16.583877253544));
#15059=CARTESIAN_POINT('Ctrl Pts',(-202.605672824408,-65.9114642758204,
16.5551712045959));
#15060=CARTESIAN_POINT('Ctrl Pts',(-202.838472376554,-66.2989195852673,
16.5264651556479));
#15061=CARTESIAN_POINT('Ctrl Pts',(-203.268042528788,-67.0138661336119,
16.4734957160465));
#15062=CARTESIAN_POINT('Ctrl Pts',(-204.087553320887,-67.4944495440329,
16.420526276445));
#15063=CARTESIAN_POINT('Ctrl Pts',(-204.92122517779,-67.5204925072279,16.3675568368436));
#15064=CARTESIAN_POINT('Ctrl Pts',(-205.754897034692,-67.5465354704228,
16.3145873972421));
#15065=CARTESIAN_POINT('Ctrl Pts',(-206.602729956398,-67.1180379863916,
16.2616179576407));
#15066=CARTESIAN_POINT('Ctrl Pts',(-207.076140556712,-66.4313628943424,
16.2086485180393));
#15067=CARTESIAN_POINT('Ctrl Pts',(-207.549551157025,-65.7446878022932,
16.1556790784378));
#15068=CARTESIAN_POINT('Ctrl Pts',(-207.648539435946,-64.799835102226,16.1027096388364));
#15069=CARTESIAN_POINT('Ctrl Pts',(-207.327701310022,-64.0299481709965,
16.049740199235));
#15070=CARTESIAN_POINT('Ctrl Pts',(-207.006863184097,-63.2600612397671,
15.9967707596335));
#15071=CARTESIAN_POINT('Ctrl Pts',(-206.266198653327,-62.6651400773755,
15.9438013200321));
#15072=CARTESIAN_POINT('Ctrl Pts',(-205.445237999217,-62.5178795321244,
15.8908318804307));
#15073=CARTESIAN_POINT('Ctrl Pts',(-204.624277345108,-62.3706189868733,
15.8378624408292));
#15074=CARTESIAN_POINT('Ctrl Pts',(-203.72302056766,-62.6710190587628,15.7848930012278));
#15075=CARTESIAN_POINT('Ctrl Pts',(-203.154592033966,-63.2813846823738,
15.7319235616264));
#15076=CARTESIAN_POINT('Ctrl Pts',(-202.727701805557,-63.7397696947918,
15.6921434752482));
#15077=CARTESIAN_POINT('Ctrl Pts',(-202.48852739089,-64.3729759156404,15.6523633888701));
#15078=CARTESIAN_POINT('Ctrl Pts',(-202.48281438265,-65.0023102366302,15.612583302492));
#15079=CARTESIAN_POINT('Origin',(-205.,-65.,9.));
#15080=CARTESIAN_POINT('',(-202.478480635384,-64.9993246233377,14.612583302492));
#15081=CARTESIAN_POINT('',(-202.483913362404,-64.9978104805478,14.887416697508));
#15082=CARTESIAN_POINT('',(-202.4825,-65.,9.));
#15083=CARTESIAN_POINT('Ctrl Pts',(-202.483913362404,-64.9978104805478,
14.887416697508));
#15084=CARTESIAN_POINT('Ctrl Pts',(-202.481864049093,-64.7508707218699,
14.9030084168533));
#15085=CARTESIAN_POINT('Ctrl Pts',(-202.51526717488,-64.5044733838642,14.9186001361987));
#15086=CARTESIAN_POINT('Ctrl Pts',(-202.586387196479,-64.2694915479097,
14.934191855544));
#15087=CARTESIAN_POINT('Ctrl Pts',(-202.828001838529,-63.4711924064649,
14.9871612951454));
#15088=CARTESIAN_POINT('Ctrl Pts',(-203.504926517813,-62.8046454284989,
15.0401307347469));
#15089=CARTESIAN_POINT('Ctrl Pts',(-204.306862945724,-62.5753909604694,
15.0931001743483));
#15090=CARTESIAN_POINT('Ctrl Pts',(-205.108799373635,-62.34613649244,15.1460696139497));
#15091=CARTESIAN_POINT('Ctrl Pts',(-206.035747550172,-62.5541745343471,
15.1990390535512));
#15092=CARTESIAN_POINT('Ctrl Pts',(-206.66279919664,-63.1041437994002,15.2520084931526));
#15093=CARTESIAN_POINT('Ctrl Pts',(-207.289850843108,-63.6541130644534,
15.3049779327541));
#15094=CARTESIAN_POINT('Ctrl Pts',(-207.617005959508,-64.5460135526525,
15.3579473723555));
#15095=CARTESIAN_POINT('Ctrl Pts',(-207.494299322538,-65.3709985580089,
15.4109168119569));
#15096=CARTESIAN_POINT('Ctrl Pts',(-207.371592685568,-66.1959835633652,
15.4638862515584));
#15097=CARTESIAN_POINT('Ctrl Pts',(-206.799024295229,-66.9540530858788,
15.5168556911598));
#15098=CARTESIAN_POINT('Ctrl Pts',(-206.039054544245,-67.2977215702459,
15.5698251307612));
#15099=CARTESIAN_POINT('Ctrl Pts',(-205.27908479326,-67.6413900546129,15.6227945703627));
#15100=CARTESIAN_POINT('Ctrl Pts',(-204.33171368163,-67.5706575008334,15.6757640099641));
#15101=CARTESIAN_POINT('Ctrl Pts',(-203.631214451117,-67.1179282170362,
15.7287334495655));
#15102=CARTESIAN_POINT('Ctrl Pts',(-202.931707377382,-66.6658401593929,
15.7816278655464));
#15103=CARTESIAN_POINT('Ctrl Pts',(-202.47837336272,-65.832836692676,15.8345222815272));
#15104=CARTESIAN_POINT('Ctrl Pts',(-202.478262929558,-64.9999671733494,
15.887416697508));
#15105=CARTESIAN_POINT('Ctrl Pts',(-202.48281438265,-65.0023102366302,15.612583302492));
#15106=CARTESIAN_POINT('Ctrl Pts',(-202.480920196627,-65.2109702323926,
15.5993939492687));
#15107=CARTESIAN_POINT('Ctrl Pts',(-202.504690383233,-65.4192045908632,
15.5862045960454));
#15108=CARTESIAN_POINT('Ctrl Pts',(-202.555792276411,-65.6205003111822,
15.5730152428221));
#15109=CARTESIAN_POINT('Ctrl Pts',(-202.761021342488,-66.4289191410472,
15.5200458032206));
#15110=CARTESIAN_POINT('Ctrl Pts',(-203.407079764582,-67.1254256254448,
15.4670763636192));
#15111=CARTESIAN_POINT('Ctrl Pts',(-204.197816390868,-67.3907466530304,
15.4141069240177));
#15112=CARTESIAN_POINT('Ctrl Pts',(-204.988553017154,-67.6560676806159,
15.3611374844163));
#15113=CARTESIAN_POINT('Ctrl Pts',(-205.923967847632,-67.4902032513894,
15.3081680448149));
#15114=CARTESIAN_POINT('Ctrl Pts',(-206.575272719714,-66.9691839307848,
15.2551986052134));
#15115=CARTESIAN_POINT('Ctrl Pts',(-207.226577591796,-66.4481646101802,
15.202229165612));
#15116=CARTESIAN_POINT('Ctrl Pts',(-207.593772505481,-65.5719903981975,
15.1492597260106));
#15117=CARTESIAN_POINT('Ctrl Pts',(-207.508536991204,-64.7422950273395,
15.0962902864091));
#15118=CARTESIAN_POINT('Ctrl Pts',(-207.423301476928,-63.9125996564815,
15.0433208468077));
#15119=CARTESIAN_POINT('Ctrl Pts',(-206.885635534689,-63.1293831267483,
14.9903514072063));
#15120=CARTESIAN_POINT('Ctrl Pts',(-206.14200240898,-62.7516673386529,14.9373819676048));
#15121=CARTESIAN_POINT('Ctrl Pts',(-205.398369283272,-62.3739515505575,
14.8844125280034));
#15122=CARTESIAN_POINT('Ctrl Pts',(-204.448768974094,-62.4017365040998,
14.831443088402));
#15123=CARTESIAN_POINT('Ctrl Pts',(-203.728492868385,-62.822285819182,14.7784736488005));
#15124=CARTESIAN_POINT('Ctrl Pts',(-203.008216762676,-63.2428351342642,
14.7255042091991));
#15125=CARTESIAN_POINT('Ctrl Pts',(-202.517264860435,-64.0561488108863,
14.6725347695977));
#15126=CARTESIAN_POINT('Ctrl Pts',(-202.480686812783,-64.889408362383,14.6195653299962));
#15127=CARTESIAN_POINT('Ctrl Pts',(-202.479079666369,-64.9260196685153,
14.6172379874948));
#15128=CARTESIAN_POINT('Ctrl Pts',(-202.478349688759,-64.9626694801625,
14.6149106449934));
#15129=CARTESIAN_POINT('Ctrl Pts',(-202.478480635384,-64.9993246233377,
14.612583302492));
#15130=CARTESIAN_POINT('Origin',(-205.,-65.,9.));
#15131=CARTESIAN_POINT('',(-202.484829278355,-64.9980759284861,13.612583302492));
#15132=CARTESIAN_POINT('',(-202.486036851904,-65.0011568554962,13.887416697508));
#15133=CARTESIAN_POINT('',(-202.4825,-65.,9.));
#15134=CARTESIAN_POINT('Ctrl Pts',(-202.486036851904,-65.0011568554962,
13.887416697508));
#15135=CARTESIAN_POINT('Ctrl Pts',(-202.488081620308,-64.5074181159925,
13.9185251125781));
#15136=CARTESIAN_POINT('Ctrl Pts',(-202.628468371682,-64.0126062150085,
13.9496335276481));
#15137=CARTESIAN_POINT('Ctrl Pts',(-202.899518826464,-63.6045975021718,
13.9807419427182));
#15138=CARTESIAN_POINT('Ctrl Pts',(-203.361046379736,-62.9098660983765,
14.0337113823196));
#15139=CARTESIAN_POINT('Ctrl Pts',(-204.201408805511,-62.4668042390463,
14.086680821921));
#15140=CARTESIAN_POINT('Ctrl Pts',(-205.035388666738,-62.4785089905249,
14.1396502615225));
#15141=CARTESIAN_POINT('Ctrl Pts',(-205.869368527965,-62.4902137420035,
14.1926197011239));
#15142=CARTESIAN_POINT('Ctrl Pts',(-206.696965824644,-62.956685104291,14.2455891407254));
#15143=CARTESIAN_POINT('Ctrl Pts',(-207.138814575472,-63.664095240497,14.2985585803268));
#15144=CARTESIAN_POINT('Ctrl Pts',(-207.580663326299,-64.3715053767029,
14.3515280199282));
#15145=CARTESIAN_POINT('Ctrl Pts',(-207.636763531275,-65.3198542868274,
14.4044974595297));
#15146=CARTESIAN_POINT('Ctrl Pts',(-207.281399181164,-66.0744240710213,
14.4574668991311));
#15147=CARTESIAN_POINT('Ctrl Pts',(-206.926034831053,-66.8289938552152,
14.5104363387325));
#15148=CARTESIAN_POINT('Ctrl Pts',(-206.159205925855,-67.3897845134786,
14.563405778334));
#15149=CARTESIAN_POINT('Ctrl Pts',(-205.33242252728,-67.4997328638535,14.6163752179354));
#15150=CARTESIAN_POINT('Ctrl Pts',(-204.505639128704,-67.6096812142285,
14.6693446575368));
#15151=CARTESIAN_POINT('Ctrl Pts',(-203.618901236752,-67.268787256715,14.7223140971383));
#15152=CARTESIAN_POINT('Ctrl Pts',(-203.078684593183,-66.6333146254965,
14.7752835367397));
#15153=CARTESIAN_POINT('Ctrl Pts',(-202.697482399372,-66.1848953403611,
14.8126612569958));
#15154=CARTESIAN_POINT('Ctrl Pts',(-202.488826140652,-65.5897942775585,
14.8500389772519));
#15155=CARTESIAN_POINT('Ctrl Pts',(-202.483913362404,-64.9978104805478,
14.887416697508));
#15156=CARTESIAN_POINT('Ctrl Pts',(-202.478480635384,-64.9993246233377,
14.612583302492));
#15157=CARTESIAN_POINT('Ctrl Pts',(-202.481329984672,-65.7969267462619,
14.561941205392));
#15158=CARTESIAN_POINT('Ctrl Pts',(-202.891810794862,-66.597053247633,14.5112991082919));
#15159=CARTESIAN_POINT('Ctrl Pts',(-203.542558949731,-67.0579200627044,
14.4606570111919));
#15160=CARTESIAN_POINT('Ctrl Pts',(-204.223213327393,-67.5399667851577,
14.4076875715905));
#15161=CARTESIAN_POINT('Ctrl Pts',(-205.166726275778,-67.6508548036931,
14.354718131989));
#15162=CARTESIAN_POINT('Ctrl Pts',(-205.940596742163,-67.3397536602911,
14.3017486923876));
#15163=CARTESIAN_POINT('Ctrl Pts',(-206.714467208547,-67.0286525168891,
14.2487792527862));
#15164=CARTESIAN_POINT('Ctrl Pts',(-207.318695192931,-66.2955622115496,
14.1958098131847));
#15165=CARTESIAN_POINT('Ctrl Pts',(-207.476305959037,-65.4765272483028,
14.1428403735833));
#15166=CARTESIAN_POINT('Ctrl Pts',(-207.633916725142,-64.657492285056,14.0898709339819));
#15167=CARTESIAN_POINT('Ctrl Pts',(-207.34491027297,-63.7525126639018,14.0369014943804));
#15168=CARTESIAN_POINT('Ctrl Pts',(-206.741765547493,-63.1764259834307,
13.983932054779));
#15169=CARTESIAN_POINT('Ctrl Pts',(-206.138620822016,-62.6003393029595,
13.9309626151776));
#15170=CARTESIAN_POINT('Ctrl Pts',(-205.221337823236,-62.3531455631714,
13.8779931755761));
#15171=CARTESIAN_POINT('Ctrl Pts',(-204.410393950494,-62.5481569941157,
13.8250237359747));
#15172=CARTESIAN_POINT('Ctrl Pts',(-203.599450077753,-62.74316842506,13.7720542963732));
#15173=CARTESIAN_POINT('Ctrl Pts',(-202.894845331051,-63.3803850267366,
13.7190848567718));
#15174=CARTESIAN_POINT('Ctrl Pts',(-202.619566589227,-64.167710269399,13.6661154171704));
#15175=CARTESIAN_POINT('Ctrl Pts',(-202.526832279993,-64.4329398401132,
13.6482713789442));
#15176=CARTESIAN_POINT('Ctrl Pts',(-202.482819703866,-64.7152043750739,
13.6304273407181));
#15177=CARTESIAN_POINT('Ctrl Pts',(-202.484829278355,-64.9980759284861,
13.612583302492));
#15178=CARTESIAN_POINT('Origin',(-205.,-65.,9.));
#15179=CARTESIAN_POINT('',(-202.485436300316,-65.0016271999185,12.612583302492));
#15180=CARTESIAN_POINT('',(-202.47967327723,-65.0016558771702,12.887416697508));
#15181=CARTESIAN_POINT('',(-202.4825,-65.,9.));
#15182=CARTESIAN_POINT('Ctrl Pts',(-202.47967327723,-65.0016558771702,12.887416697508));
#15183=CARTESIAN_POINT('Ctrl Pts',(-202.485262109409,-64.2664021257915,
12.9340418083028));
#15184=CARTESIAN_POINT('Ctrl Pts',(-202.825745335394,-63.5266425796602,
12.9806669190976));
#15185=CARTESIAN_POINT('Ctrl Pts',(-203.391061346414,-63.0582261468577,
13.0272920298923));
#15186=CARTESIAN_POINT('Ctrl Pts',(-204.033300513057,-62.5260717879144,
13.0802614694938));
#15187=CARTESIAN_POINT('Ctrl Pts',(-204.965721795584,-62.3441284479905,
13.1332309090952));
#15188=CARTESIAN_POINT('Ctrl Pts',(-205.760908488858,-62.5957979371522,
13.1862003486966));
#15189=CARTESIAN_POINT('Ctrl Pts',(-206.556095182133,-62.8474674263139,
13.2391697882981));
#15190=CARTESIAN_POINT('Ctrl Pts',(-207.214047286156,-63.5327497445611,
13.2921392278995));
#15191=CARTESIAN_POINT('Ctrl Pts',(-207.433163233268,-64.3375153072165,
13.3451086675009));
#15192=CARTESIAN_POINT('Ctrl Pts',(-207.652279180381,-65.1422808698718,
13.3980781071024));
#15193=CARTESIAN_POINT('Ctrl Pts',(-207.432558970583,-66.0665296769353,
13.4510475467038));
#15194=CARTESIAN_POINT('Ctrl Pts',(-206.87472112031,-66.6865912395403,13.5040169863053));
#15195=CARTESIAN_POINT('Ctrl Pts',(-206.316883270037,-67.3066528021453,
13.5569864259067));
#15196=CARTESIAN_POINT('Ctrl Pts',(-205.420927779289,-67.6225271202918,
13.6099558655081));
#15197=CARTESIAN_POINT('Ctrl Pts',(-204.597555637766,-67.4894191733733,
13.6629253051096));
#15198=CARTESIAN_POINT('Ctrl Pts',(-203.774183496244,-67.3563112264548,
13.715894744711));
#15199=CARTESIAN_POINT('Ctrl Pts',(-203.023394703947,-66.7742210144714,
13.7688641843124));
#15200=CARTESIAN_POINT('Ctrl Pts',(-202.689346648184,-66.0099754343495,
13.8218336239139));
#15201=CARTESIAN_POINT('Ctrl Pts',(-202.551481630229,-65.6945635383438,
13.8436946484453));
#15202=CARTESIAN_POINT('Ctrl Pts',(-202.484599918132,-65.348125181336,13.8655556729766));
#15203=CARTESIAN_POINT('Ctrl Pts',(-202.486036851904,-65.0011568554962,
13.887416697508));
#15204=CARTESIAN_POINT('Ctrl Pts',(-202.484829278355,-64.9980759284861,
13.612583302492));
#15205=CARTESIAN_POINT('Ctrl Pts',(-202.488785059531,-65.554899262159,13.5774579011167));
#15206=CARTESIAN_POINT('Ctrl Pts',(-202.671070348432,-66.1140747088951,
13.5423324997414));
#15207=CARTESIAN_POINT('Ctrl Pts',(-203.011093973612,-66.5502974671019,
13.5072070983661));
#15208=CARTESIAN_POINT('Ctrl Pts',(-203.523852836765,-67.2081255384944,
13.4542376587646));
#15209=CARTESIAN_POINT('Ctrl Pts',(-204.395323300017,-67.5863477976313,
13.4012682191632));
#15210=CARTESIAN_POINT('Ctrl Pts',(-205.226028173268,-67.5115892744489,
13.3482987795618));
#15211=CARTESIAN_POINT('Ctrl Pts',(-206.056733046519,-67.4368307512664,
13.2953293399603));
#15212=CARTESIAN_POINT('Ctrl Pts',(-206.846672329768,-66.9090914457645,
13.2423599003589));
#15213=CARTESIAN_POINT('Ctrl Pts',(-207.233742270005,-66.1702841064326,
13.1893904607575));
#15214=CARTESIAN_POINT('Ctrl Pts',(-207.620812210242,-65.4314767671007,
13.136421021156));
#15215=CARTESIAN_POINT('Ctrl Pts',(-207.605012807466,-64.4816013939387,
13.0834515815546));
#15216=CARTESIAN_POINT('Ctrl Pts',(-207.193586419647,-63.7560755496928,
13.0304821419532));
#15217=CARTESIAN_POINT('Ctrl Pts',(-206.782160031828,-63.030549705447,12.9775127023517));
#15218=CARTESIAN_POINT('Ctrl Pts',(-205.975106658967,-62.5293733901171,
12.9245432627503));
#15219=CARTESIAN_POINT('Ctrl Pts',(-205.142375057033,-62.4822830258936,
12.8715738231488));
#15220=CARTESIAN_POINT('Ctrl Pts',(-204.309643455099,-62.43519266167,12.8186043835474));
#15221=CARTESIAN_POINT('Ctrl Pts',(-203.451233624093,-62.8421882485527,
12.765634943946));
#15222=CARTESIAN_POINT('Ctrl Pts',(-202.960635833421,-63.5167052839601,
12.7126655043445));
#15223=CARTESIAN_POINT('Ctrl Pts',(-202.65165196471,-63.9415235099572,12.6793047703937));
#15224=CARTESIAN_POINT('Ctrl Pts',(-202.48856510167,-64.4724572895867,12.6459440364428));
#15225=CARTESIAN_POINT('Ctrl Pts',(-202.485436300316,-65.0016271999185,
12.612583302492));
#15226=CARTESIAN_POINT('Origin',(-205.,-65.,9.));
#15227=CARTESIAN_POINT('',(-202.478899831684,-65.0011462762536,11.612583302492));
#15228=CARTESIAN_POINT('',(-202.480895630158,-64.9978964133877,11.887416697508));
#15229=CARTESIAN_POINT('',(-202.4825,-65.,9.));
#15230=CARTESIAN_POINT('Ctrl Pts',(-202.480895630158,-64.9978964133877,
11.887416697508));
#15231=CARTESIAN_POINT('Ctrl Pts',(-202.479598437047,-64.8530702325355,
11.8965890644261));
#15232=CARTESIAN_POINT('Ctrl Pts',(-202.491010825932,-64.7084483834877,
11.9057614313441));
#15233=CARTESIAN_POINT('Ctrl Pts',(-202.51585765942,-64.566172707857,11.9149337982622));
#15234=CARTESIAN_POINT('Ctrl Pts',(-202.659345469871,-63.7445458721226,
11.9679032378636));
#15235=CARTESIAN_POINT('Ctrl Pts',(-203.25086383697,-63.001162492897,12.020872677465));
#15236=CARTESIAN_POINT('Ctrl Pts',(-204.019264046879,-62.6767853568972,
12.0738421170665));
#15237=CARTESIAN_POINT('Ctrl Pts',(-204.787664256787,-62.3524082208974,
12.1268115566679));
#15238=CARTESIAN_POINT('Ctrl Pts',(-205.732946309504,-62.4470373281234,
12.1797809962694));
#15239=CARTESIAN_POINT('Ctrl Pts',(-206.421798194676,-62.9172952246455,
12.2327504358708));
#15240=CARTESIAN_POINT('Ctrl Pts',(-207.110650079848,-63.3875531211675,
12.2857198754722));
#15241=CARTESIAN_POINT('Ctrl Pts',(-207.543071797474,-64.2334398069855,
12.3386893150737));
#15242=CARTESIAN_POINT('Ctrl Pts',(-207.520843648739,-65.0672055524758,
12.3916587546751));
#15243=CARTESIAN_POINT('Ctrl Pts',(-207.498615500004,-65.9009712979661,
12.4446281942765));
#15244=CARTESIAN_POINT('Ctrl Pts',(-207.021737484906,-66.7226161031286,
12.497597633878));
#15245=CARTESIAN_POINT('Ctrl Pts',(-206.308807820586,-67.1555025809437,
12.5505670734794));
#15246=CARTESIAN_POINT('Ctrl Pts',(-205.595878156265,-67.5883890587588,
12.6035365130808));
#15247=CARTESIAN_POINT('Ctrl Pts',(-204.646896842722,-67.6325172092266,
12.6565059526823));
#15248=CARTESIAN_POINT('Ctrl Pts',(-203.896871610796,-67.2676589347991,
12.7094753922837));
#15249=CARTESIAN_POINT('Ctrl Pts',(-203.14684637887,-66.9028006603717,12.7624448318852));
#15250=CARTESIAN_POINT('Ctrl Pts',(-202.595777228561,-66.1289559610491,
12.8154142714866));
#15251=CARTESIAN_POINT('Ctrl Pts',(-202.496271178786,-65.3008509224064,
12.868383711088));
#15252=CARTESIAN_POINT('Ctrl Pts',(-202.484353002895,-65.2016659831068,
12.8747280398947));
#15253=CARTESIAN_POINT('Ctrl Pts',(-202.478912798845,-65.1017026432918,
12.8810723687013));
#15254=CARTESIAN_POINT('Ctrl Pts',(-202.47967327723,-65.0016558771702,12.887416697508));
#15255=CARTESIAN_POINT('Ctrl Pts',(-202.485436300316,-65.0016271999185,
12.612583302492));
#15256=CARTESIAN_POINT('Ctrl Pts',(-202.483597259698,-65.3126616341767,
12.5929745968414));
#15257=CARTESIAN_POINT('Ctrl Pts',(-202.537021007432,-65.6230866816078,
12.5733658911908));
#15258=CARTESIAN_POINT('Ctrl Pts',(-202.64856288418,-65.9109955592103,12.5537571855402));
#15259=CARTESIAN_POINT('Ctrl Pts',(-202.949873475951,-66.6887303151208,
12.5007877459388));
#15260=CARTESIAN_POINT('Ctrl Pts',(-203.675280409832,-67.3021613430098,
12.4478183063374));
#15261=CARTESIAN_POINT('Ctrl Pts',(-204.492261201195,-67.4700952877871,
12.3948488667359));
#15262=CARTESIAN_POINT('Ctrl Pts',(-205.309241992558,-67.6380292325644,
12.3418794271345));
#15263=CARTESIAN_POINT('Ctrl Pts',(-206.217796641404,-67.36046609423,12.288909987533));
#15264=CARTESIAN_POINT('Ctrl Pts',(-206.801448774064,-66.7646392642643,
12.2359405479316));
#15265=CARTESIAN_POINT('Ctrl Pts',(-207.385100906723,-66.1688124342986,
12.1829711083302));
#15266=CARTESIAN_POINT('Ctrl Pts',(-207.643850523198,-65.2547219127016,
12.1300016687287));
#15267=CARTESIAN_POINT('Ctrl Pts',(-207.459088245291,-64.4413816862725,
12.0770322291273));
#15268=CARTESIAN_POINT('Ctrl Pts',(-207.274325967383,-63.6280414598435,
12.0240627895259));
#15269=CARTESIAN_POINT('Ctrl Pts',(-206.646051795095,-62.9154515285825,
11.9710933499244));
#15270=CARTESIAN_POINT('Ctrl Pts',(-205.862263097956,-62.6302591347446,
11.918123910323));
#15271=CARTESIAN_POINT('Ctrl Pts',(-205.078474400818,-62.3450667409066,
11.8651544707216));
#15272=CARTESIAN_POINT('Ctrl Pts',(-204.13917117883,-62.4872718844917,11.8121850311201));
#15273=CARTESIAN_POINT('Ctrl Pts',(-203.474924779752,-62.9916885223792,
11.7592155915187));
#15274=CARTESIAN_POINT('Ctrl Pts',(-202.861992928812,-63.4571378254309,
11.7103381618431));
#15275=CARTESIAN_POINT('Ctrl Pts',(-202.483261883573,-64.2309969432331,
11.6614607321676));
#15276=CARTESIAN_POINT('Ctrl Pts',(-202.478899831684,-65.0011462762536,
11.612583302492));
#15277=CARTESIAN_POINT('Origin',(-205.,-65.,9.));
#15278=CARTESIAN_POINT('',(-202.481967477543,-64.9977164154893,10.612583302492));
#15279=CARTESIAN_POINT('',(-202.486473126263,-64.9995333153038,10.887416697508));
#15280=CARTESIAN_POINT('',(-202.4825,-65.,9.));
#15281=CARTESIAN_POINT('Ctrl Pts',(-202.486473126263,-64.9995333153038,
10.887416697508));
#15282=CARTESIAN_POINT('Ctrl Pts',(-202.485824907356,-64.6075097677981,
10.9121057601508));
#15283=CARTESIAN_POINT('Ctrl Pts',(-202.57198392834,-64.2157559153882,10.9367948227936));
#15284=CARTESIAN_POINT('Ctrl Pts',(-202.746442451943,-63.8683429559854,
10.9614838854363));
#15285=CARTESIAN_POINT('Ctrl Pts',(-203.120736541707,-63.1229817393159,
11.0144533250378));
#15286=CARTESIAN_POINT('Ctrl Pts',(-203.901473783378,-62.5817219250026,
11.0674227646392));
#15287=CARTESIAN_POINT('Ctrl Pts',(-204.730768588446,-62.4926739871521,
11.1203922042406));
#15288=CARTESIAN_POINT('Ctrl Pts',(-205.560063393513,-62.4036260493017,
11.1733616438421));
#15289=CARTESIAN_POINT('Ctrl Pts',(-206.437915761975,-62.7667899879141,
11.2263310834435));
#15290=CARTESIAN_POINT('Ctrl Pts',(-206.961923073917,-63.4156934830335,
11.279300523045));
#15291=CARTESIAN_POINT('Ctrl Pts',(-207.485930385859,-64.0645969781529,
11.3322699626464));
#15292=CARTESIAN_POINT('Ctrl Pts',(-207.65609264128,-64.9992400297792,11.3852394022478));
#15293=CARTESIAN_POINT('Ctrl Pts',(-207.39440841323,-65.7911874862032,11.4382088418493));
#15294=CARTESIAN_POINT('Ctrl Pts',(-207.13272418518,-66.5831349426273,11.4911782814507));
#15295=CARTESIAN_POINT('Ctrl Pts',(-206.439193473658,-67.2323868038489,
11.5441477210521));
#15296=CARTESIAN_POINT('Ctrl Pts',(-205.631726881101,-67.441329644961,11.5971171606536));
#15297=CARTESIAN_POINT('Ctrl Pts',(-204.824260288545,-67.650272486073,11.650086600255));
#15298=CARTESIAN_POINT('Ctrl Pts',(-203.902857814954,-67.4189063070754,
11.7030560398564));
#15299=CARTESIAN_POINT('Ctrl Pts',(-203.28988520506,-66.853288071455,11.7560254794579));
#15300=CARTESIAN_POINT('Ctrl Pts',(-202.783057000902,-66.3856141983139,
11.7998225521413));
#15301=CARTESIAN_POINT('Ctrl Pts',(-202.487089588759,-65.6894259636016,
11.8436196248246));
#15302=CARTESIAN_POINT('Ctrl Pts',(-202.480895630158,-64.9978964133877,
11.887416697508));
#15303=CARTESIAN_POINT('Ctrl Pts',(-202.478899831684,-65.0011462762536,
11.612583302492));
#15304=CARTESIAN_POINT('Ctrl Pts',(-202.478534641458,-65.0656230446933,
11.6084912925661));
#15305=CARTESIAN_POINT('Ctrl Pts',(-202.480793406997,-65.1300738112168,
11.6043992826403));
#15306=CARTESIAN_POINT('Ctrl Pts',(-202.485758378021,-65.1943154262143,
11.6003072727144));
#15307=CARTESIAN_POINT('Ctrl Pts',(-202.550027951534,-66.0258975599723,
11.547337833113));
#15308=CARTESIAN_POINT('Ctrl Pts',(-203.067756674727,-66.8224336952987,
11.4943683935115));
#15309=CARTESIAN_POINT('Ctrl Pts',(-203.801620594161,-67.2187961191196,
11.4413989539101));
#15310=CARTESIAN_POINT('Ctrl Pts',(-204.535484513596,-67.6151585429404,
11.3884295143086));
#15311=CARTESIAN_POINT('Ctrl Pts',(-205.485483629272,-67.6113472552559,
11.3354600747072));
#15312=CARTESIAN_POINT('Ctrl Pts',(-206.216143655536,-67.2091093290415,
11.2824906351058));
#15313=CARTESIAN_POINT('Ctrl Pts',(-206.9468036818,-66.8068714028271,11.2295211955043));
#15314=CARTESIAN_POINT('Ctrl Pts',(-207.458124618651,-66.0062068380828,
11.1765517559029));
#15315=CARTESIAN_POINT('Ctrl Pts',(-207.515719806102,-65.1741357968564,
11.1235823163015));
#15316=CARTESIAN_POINT('Ctrl Pts',(-207.573314993552,-64.3420647556299,
11.0706128767));
#15317=CARTESIAN_POINT('Ctrl Pts',(-207.177184431601,-63.4785872379213,
11.0176434370986));
#15318=CARTESIAN_POINT('Ctrl Pts',(-206.508912156113,-62.9795165123932,
10.9646739974972));
#15319=CARTESIAN_POINT('Ctrl Pts',(-205.840639880625,-62.4804457868651,
10.9117045578957));
#15320=CARTESIAN_POINT('Ctrl Pts',(-204.9002258916,-62.3457818535176,10.8587351182943));
#15321=CARTESIAN_POINT('Ctrl Pts',(-204.1187507062,-62.6372539068417,10.8057656786929));
#15322=CARTESIAN_POINT('Ctrl Pts',(-203.3372755208,-62.9287259601658,10.7527962390914));
#15323=CARTESIAN_POINT('Ctrl Pts',(-202.714739139025,-63.6463340001615,
10.69982679949));
#15324=CARTESIAN_POINT('Ctrl Pts',(-202.536508759301,-64.4611305115731,
10.6468573598885));
#15325=CARTESIAN_POINT('Ctrl Pts',(-202.498067233329,-64.6368694697899,
10.6354326740897));
#15326=CARTESIAN_POINT('Ctrl Pts',(-202.480294730592,-64.8171296155769,
10.6240079882908));
#15327=CARTESIAN_POINT('Ctrl Pts',(-202.481967477543,-64.9977164154893,
10.612583302492));
#15328=CARTESIAN_POINT('Origin',(-205.,-65.,9.));
#15329=CARTESIAN_POINT('',(-202.48654680791,-65.0001194272881,9.61258330249198));
#15330=CARTESIAN_POINT('',(-202.482611587334,-65.0023130412151,9.88741669750802));
#15331=CARTESIAN_POINT('',(-202.4825,-65.,9.));
#15332=CARTESIAN_POINT('Ctrl Pts',(-202.482611587334,-65.0023130412151,
9.88741669750802));
#15333=CARTESIAN_POINT('Ctrl Pts',(-202.488432663582,-64.3663757716566,
9.92762245587551));
#15334=CARTESIAN_POINT('Ctrl Pts',(-202.73327779399,-63.7264479410027,9.96782821424301));
#15335=CARTESIAN_POINT('Ctrl Pts',(-203.168440123924,-63.2666339947897,
10.0080339726105));
#15336=CARTESIAN_POINT('Ctrl Pts',(-203.741748666983,-62.6608479571479,
10.0610034122119));
#15337=CARTESIAN_POINT('Ctrl Pts',(-204.645390451181,-62.3676852839176,
10.1139728518134));
#15338=CARTESIAN_POINT('Ctrl Pts',(-205.46514113255,-62.5215301061983,10.1669422914148));
#15339=CARTESIAN_POINT('Ctrl Pts',(-206.284891813918,-62.675374928479,10.2199117310162));
#15340=CARTESIAN_POINT('Ctrl Pts',(-207.020751392457,-63.2762272462707,
10.2728811706177));
#15341=CARTESIAN_POINT('Ctrl Pts',(-207.33540594964,-64.0486597148988,10.3258506102191));
#15342=CARTESIAN_POINT('Ctrl Pts',(-207.650060506823,-64.8210921835268,
10.3788200498206));
#15343=CARTESIAN_POINT('Ctrl Pts',(-207.543510042649,-65.7651048029912,
10.431789489422));
#15344=CARTESIAN_POINT('Ctrl Pts',(-207.06459669445,-66.4479674640464,10.4847589290234));
#15345=CARTESIAN_POINT('Ctrl Pts',(-206.585683346251,-67.1308301251015,
10.5377283686249));
#15346=CARTESIAN_POINT('Ctrl Pts',(-205.734407114026,-67.5525428277475,
10.5906978082263));
#15347=CARTESIAN_POINT('Ctrl Pts',(-204.900988265359,-67.5197948257892,
10.6436672478277));
#15348=CARTESIAN_POINT('Ctrl Pts',(-204.067569416691,-67.4870468238309,
10.6966366874292));
#15349=CARTESIAN_POINT('Ctrl Pts',(-203.25200795158,-66.9998381172684,10.7496061270306));
#15350=CARTESIAN_POINT('Ctrl Pts',(-202.828152687953,-66.2815024544743,
10.802575566632));
#15351=CARTESIAN_POINT('Ctrl Pts',(-202.601856417471,-65.8979831369297,
10.8308559435907));
#15352=CARTESIAN_POINT('Ctrl Pts',(-202.487215636228,-65.4485812949919,
10.8591363205494));
#15353=CARTESIAN_POINT('Ctrl Pts',(-202.486473126263,-64.9995333153038,
10.887416697508));
#15354=CARTESIAN_POINT('Ctrl Pts',(-202.481967477543,-64.9977164154893,
10.612583302492));
#15355=CARTESIAN_POINT('Ctrl Pts',(-202.488050258416,-65.6544026714131,
10.5710385486894));
#15356=CARTESIAN_POINT('Ctrl Pts',(-202.75126577681,-66.3154084126017,10.5294937948868));
#15357=CARTESIAN_POINT('Ctrl Pts',(-203.212768047943,-66.7790366404615,
10.4879490410842));
#15358=CARTESIAN_POINT('Ctrl Pts',(-203.801182093982,-67.3701612751106,
10.4349796014828));
#15359=CARTESIAN_POINT('Ctrl Pts',(-204.711934563733,-67.6404255615813,
10.3820101618814));
#15360=CARTESIAN_POINT('Ctrl Pts',(-205.527541614709,-67.4659418612995,
10.3290407222799));
#15361=CARTESIAN_POINT('Ctrl Pts',(-206.343148665684,-67.2914581610176,
10.2760712826785));
#15362=CARTESIAN_POINT('Ctrl Pts',(-207.063610297884,-66.6722264739832,
10.2231018430771));
#15363=CARTESIAN_POINT('Ctrl Pts',(-207.358670925333,-65.8920991450205,
10.1701324034756));
#15364=CARTESIAN_POINT('Ctrl Pts',(-207.653731552782,-65.1119718160577,
10.1171629638742));
#15365=CARTESIAN_POINT('Ctrl Pts',(-207.523391175481,-64.1709488451667,
10.0641935242728));
#15366=CARTESIAN_POINT('Ctrl Pts',(-207.027397093989,-63.5003899033944,
10.0112240846713));
#15367=CARTESIAN_POINT('Ctrl Pts',(-206.531403012498,-62.829830961622,9.95825464506989));
#15368=CARTESIAN_POINT('Ctrl Pts',(-205.669755226818,-62.4297360489682,
9.90528520546845));
#15369=CARTESIAN_POINT('Ctrl Pts',(-204.837428266674,-62.4835064375044,
9.85231576586702));
#15370=CARTESIAN_POINT('Ctrl Pts',(-204.005101306531,-62.5372768260406,
9.79934632626558));
#15371=CARTESIAN_POINT('Ctrl Pts',(-203.202095171924,-63.0449125157668,
9.74637688666414));
#15372=CARTESIAN_POINT('Ctrl Pts',(-202.796503387442,-63.7737161433821,
9.69340744706271));
#15373=CARTESIAN_POINT('Ctrl Pts',(-202.590210795132,-64.1444011409031,
9.66646606553913));
#15374=CARTESIAN_POINT('Ctrl Pts',(-202.486727528942,-64.5723013010034,
9.63952468401556));
#15375=CARTESIAN_POINT('Ctrl Pts',(-202.48654680791,-65.0001194272881,9.61258330249198));
#15376=CARTESIAN_POINT('Origin',(-205.,-65.,9.));
#15377=CARTESIAN_POINT('',(-202.481528147891,-65.0022302324439,8.61258330249198));
#15378=CARTESIAN_POINT('',(-202.478564020843,-64.9992065504904,8.88741669750802));
#15379=CARTESIAN_POINT('',(-202.4825,-65.,9.));
#15380=CARTESIAN_POINT('Ctrl Pts',(-202.478564020843,-64.9992065504904,
8.88741669750802));
#15381=CARTESIAN_POINT('Ctrl Pts',(-202.478385164604,-64.9558433406332,
8.8901697119988));
#15382=CARTESIAN_POINT('Ctrl Pts',(-202.479406771777,-64.9124887333215,
8.89292272648958));
#15383=CARTESIAN_POINT('Ctrl Pts',(-202.481655288571,-64.8691978513664,
8.89567574098036));
#15384=CARTESIAN_POINT('Ctrl Pts',(-202.52491792845,-64.03625862613,8.94864518058179));
#15385=CARTESIAN_POINT('Ctrl Pts',(-203.022379735769,-63.2269103837877,
9.00161462018323));
#15386=CARTESIAN_POINT('Ctrl Pts',(-203.746006998067,-62.8121538356702,
9.05458405978466));
#15387=CARTESIAN_POINT('Ctrl Pts',(-204.469634260364,-62.3973972875527,
9.1075534993861));
#15388=CARTESIAN_POINT('Ctrl Pts',(-205.41942697764,-62.3772324336601,9.16052293898754));
#15389=CARTESIAN_POINT('Ctrl Pts',(-206.160005476114,-62.7609027303274,
9.21349237858897));
#15390=CARTESIAN_POINT('Ctrl Pts',(-206.900583974588,-63.1445730269947,
9.26646181819041));
#15391=CARTESIAN_POINT('Ctrl Pts',(-207.43194825426,-63.932078474222,9.31943125779184));
#15392=CARTESIAN_POINT('Ctrl Pts',(-207.510523898802,-64.7624309758931,
9.37240069739327));
#15393=CARTESIAN_POINT('Ctrl Pts',(-207.589099543344,-65.5927834775642,
9.42537013699471));
#15394=CARTESIAN_POINT('Ctrl Pts',(-207.214886552757,-66.4659830336792,
9.47833957659615));
#15395=CARTESIAN_POINT('Ctrl Pts',(-206.559422070674,-66.9817598475003,
9.53130901619758));
#15396=CARTESIAN_POINT('Ctrl Pts',(-205.903957588592,-67.4975366613213,
9.58427845579902));
#15397=CARTESIAN_POINT('Ctrl Pts',(-204.967241615015,-67.6558907328485,
9.63724789540045));
#15398=CARTESIAN_POINT('Ctrl Pts',(-204.178659517491,-67.3842334406392,
9.69021733500189));
#15399=CARTESIAN_POINT('Ctrl Pts',(-203.390077419966,-67.1125761484299,
9.74318677460333));
#15400=CARTESIAN_POINT('Ctrl Pts',(-202.749629198494,-66.410907492484,9.79615621420476));
#15401=CARTESIAN_POINT('Ctrl Pts',(-202.550892738719,-65.6008684634844,
9.8491256538062));
#15402=CARTESIAN_POINT('Ctrl Pts',(-202.503004582053,-65.4056789347486,
9.86188933504014));
#15403=CARTESIAN_POINT('Ctrl Pts',(-202.480763634088,-65.2041970728315,
9.87465301627408));
#15404=CARTESIAN_POINT('Ctrl Pts',(-202.482611587334,-65.0023130412151,
9.88741669750802));
#15405=CARTESIAN_POINT('Ctrl Pts',(-202.48654680791,-65.0001194272881,9.61258330249198));
#15406=CARTESIAN_POINT('Ctrl Pts',(-202.486372213392,-65.4134343505764,
9.58655524441412));
#15407=CARTESIAN_POINT('Ctrl Pts',(-202.582614889168,-65.8266727077302,
9.56052718633626));
#15408=CARTESIAN_POINT('Ctrl Pts',(-202.775719574576,-66.188169183086,9.5344991282584));
#15409=CARTESIAN_POINT('Ctrl Pts',(-203.168704980553,-66.9238470296702,
9.48152968865696));
#15410=CARTESIAN_POINT('Ctrl Pts',(-203.962853226864,-67.4452311573341,
9.42856024905553));
#15411=CARTESIAN_POINT('Ctrl Pts',(-204.794131195417,-67.5133219956579,
9.37559080945409));
#15412=CARTESIAN_POINT('Ctrl Pts',(-205.62540916397,-67.5814128339818,9.32262136985265));
#15413=CARTESIAN_POINT('Ctrl Pts',(-206.493816854764,-67.1962103829656,
9.26965193025122));
#15414=CARTESIAN_POINT('Ctrl Pts',(-207.001281035346,-66.534289293491,9.21668249064978));
#15415=CARTESIAN_POINT('Ctrl Pts',(-207.508745215928,-65.8723682040165,
9.16371305104835));
#15416=CARTESIAN_POINT('Ctrl Pts',(-207.655265886299,-64.9337284760836,
9.11074361144692));
#15417=CARTESIAN_POINT('Ctrl Pts',(-207.373678789975,-64.1486373154858,
9.05777417184549));
#15418=CARTESIAN_POINT('Ctrl Pts',(-207.092091693651,-63.3635461548879,
9.00480473224405));
#15419=CARTESIAN_POINT('Ctrl Pts',(-206.382396830632,-62.7320035616251,
8.95183529264261));
#15420=CARTESIAN_POINT('Ctrl Pts',(-205.569914360071,-62.5435051311385,
8.89886585304118));
#15421=CARTESIAN_POINT('Ctrl Pts',(-204.75743188951,-62.3550067006518,8.84589641343974));
#15422=CARTESIAN_POINT('Ctrl Pts',(-203.842161811406,-62.6095524329414,
8.79292697383831));
#15423=CARTESIAN_POINT('Ctrl Pts',(-203.243658814669,-63.1904599868281,
8.73995753423687));
#15424=CARTESIAN_POINT('Ctrl Pts',(-202.763923958874,-63.6560910749164,
8.69749945698857));
#15425=CARTESIAN_POINT('Ctrl Pts',(-202.487710433184,-64.3314080676777,
8.65504137974028));
#15426=CARTESIAN_POINT('Ctrl Pts',(-202.481528147891,-65.0022302324439,
8.61258330249198));
#15427=CARTESIAN_POINT('Origin',(-205.,-65.,9.));
#15428=CARTESIAN_POINT('',(-202.479185579191,-64.9986328469134,7.61258330249198));
#15429=CARTESIAN_POINT('',(-202.484985611247,-64.9981409264881,7.88741669750801));
#15430=CARTESIAN_POINT('',(-202.4825,-65.,9.));
#15431=CARTESIAN_POINT('Ctrl Pts',(-202.484985611247,-64.9981409264881,
7.88741669750801));
#15432=CARTESIAN_POINT('Ctrl Pts',(-202.483005664854,-64.7084761452466,
7.90568640772351));
#15433=CARTESIAN_POINT('Ctrl Pts',(-202.529198919473,-64.4194234219896,
7.92395611793902));
#15434=CARTESIAN_POINT('Ctrl Pts',(-202.626321234454,-64.1486373242474,
7.94222582815452));
#15435=CARTESIAN_POINT('Ctrl Pts',(-202.90790832788,-63.3635461717291,7.99519526775595));
#15436=CARTESIAN_POINT('Ctrl Pts',(-203.617603183594,-62.7320035849656,
8.04816470735739));
#15437=CARTESIAN_POINT('Ctrl Pts',(-204.430085645794,-62.5435051564189,
8.10113414695882));
#15438=CARTESIAN_POINT('Ctrl Pts',(-205.242568107994,-62.3550067278721,
8.15410358656026));
#15439=CARTESIAN_POINT('Ctrl Pts',(-206.157838176679,-62.6095524575421,
8.20707302616169));
#15440=CARTESIAN_POINT('Ctrl Pts',(-206.756341167256,-63.1904600054505,
8.26004246576313));
#15441=CARTESIAN_POINT('Ctrl Pts',(-207.354844157833,-63.771367553359,8.31301190536457));
#15442=CARTESIAN_POINT('Ctrl Pts',(-207.636580070302,-64.6786369195059,
8.365981344966));
#15443=CARTESIAN_POINT('Ctrl Pts',(-207.472402736839,-65.4963808966307,
8.41895078456743));
#15444=CARTESIAN_POINT('Ctrl Pts',(-207.308225403377,-66.3141248737555,
8.47192022416887));
#15445=CARTESIAN_POINT('Ctrl Pts',(-206.698134823983,-67.0423434618581,
8.52488966377031));
#15446=CARTESIAN_POINT('Ctrl Pts',(-205.921793110823,-67.3472253297266,
8.57785910337174));
#15447=CARTESIAN_POINT('Ctrl Pts',(-205.145451397663,-67.652107197595,8.63082854297318));
#15448=CARTESIAN_POINT('Ctrl Pts',(-204.202858550738,-67.5336523452293,
8.68379798257461));
#15449=CARTESIAN_POINT('Ctrl Pts',(-203.526093863495,-67.0461598149813,
8.73676742217605));
#15450=CARTESIAN_POINT('Ctrl Pts',(-202.88450309927,-66.5840040451373,8.7869838472867));
#15451=CARTESIAN_POINT('Ctrl Pts',(-202.481826452252,-65.790174192559,8.83720027239736));
#15452=CARTESIAN_POINT('Ctrl Pts',(-202.478564020843,-64.9992065504904,
8.88741669750802));
#15453=CARTESIAN_POINT('Ctrl Pts',(-202.481528147891,-65.0022302324439,
8.61258330249198));
#15454=CARTESIAN_POINT('Ctrl Pts',(-202.479997597166,-65.168305931236,8.60207194013884));
#15455=CARTESIAN_POINT('Ctrl Pts',(-202.495017556434,-65.3341061371053,
8.5915605777857));
#15456=CARTESIAN_POINT('Ctrl Pts',(-202.527597237717,-65.4963809017392,
8.58104921543256));
#15457=CARTESIAN_POINT('Ctrl Pts',(-202.691774572869,-66.3141248872796,
8.52807977583112));
#15458=CARTESIAN_POINT('Ctrl Pts',(-203.301865158541,-67.0423434828765,
8.47511033622969));
#15459=CARTESIAN_POINT('Ctrl Pts',(-204.078206879691,-67.3472253538825,
8.42214089662826));
#15460=CARTESIAN_POINT('Ctrl Pts',(-204.85454860084,-67.6521072248885,8.36917145702682));
#15461=CARTESIAN_POINT('Ctrl Pts',(-205.797141457466,-67.5336523713038,
8.31620201742538));
#15462=CARTESIAN_POINT('Ctrl Pts',(-206.473906151673,-67.0461598360388,
8.26323257782395));
#15463=CARTESIAN_POINT('Ctrl Pts',(-207.150670845881,-66.5586673007738,
8.21026313822251));
#15464=CARTESIAN_POINT('Ctrl Pts',(-207.561607377671,-65.7021370838286,
8.15729369862108));
#15465=CARTESIAN_POINT('Ctrl Pts',(-207.518344737346,-64.8691978500202,
8.10432425901964));
#15466=CARTESIAN_POINT('Ctrl Pts',(-207.475082097022,-64.0362586162118,
8.05135481941821));
#15467=CARTESIAN_POINT('Ctrl Pts',(-206.977620284583,-63.2269103655403,
7.99838537981677));
#15468=CARTESIAN_POINT('Ctrl Pts',(-206.253993014839,-62.8121538131544,
7.94541594021533));
#15469=CARTESIAN_POINT('Ctrl Pts',(-205.530365745094,-62.3973972607686,
7.89244650061389));
#15470=CARTESIAN_POINT('Ctrl Pts',(-204.580573018043,-62.3772324066685,
7.83947706101246));
#15471=CARTESIAN_POINT('Ctrl Pts',(-203.839994511948,-62.7609027072843,
7.78650762141103));
#15472=CARTESIAN_POINT('Ctrl Pts',(-203.099416005852,-63.1445730079001,
7.7335381818096));
#15473=CARTESIAN_POINT('Ctrl Pts',(-202.568051720712,-63.9320784632318,
7.68056874220816));
#15474=CARTESIAN_POINT('Ctrl Pts',(-202.489476075362,-64.7624309734483,
7.62759930260672));
#15475=CARTESIAN_POINT('Ctrl Pts',(-202.48205109026,-64.8408949172022,7.62259396923514));
#15476=CARTESIAN_POINT('Ctrl Pts',(-202.478669170703,-64.9197414532653,
7.61758863586356));
#15477=CARTESIAN_POINT('Ctrl Pts',(-202.479185579191,-64.9986328469134,
7.61258330249198));
#15478=CARTESIAN_POINT('Origin',(-205.,-65.,9.));
#15479=CARTESIAN_POINT('',(-202.485704986804,-64.9985525930702,6.61258330249198));
#15480=CARTESIAN_POINT('',(-202.485300085822,-65.0017052192927,6.88741669750801));
#15481=CARTESIAN_POINT('',(-202.4825,-65.,9.));
#15482=CARTESIAN_POINT('Ctrl Pts',(-202.485300085822,-65.0017052192927,
6.88741669750801));
#15483=CARTESIAN_POINT('Ctrl Pts',(-202.488631949774,-64.465856140259,6.92120310344824));
#15484=CARTESIAN_POINT('Ctrl Pts',(-202.656234520208,-63.9281040224856,
6.95498950938846));
#15485=CARTESIAN_POINT('Ctrl Pts',(-202.972602926875,-63.5003899188273,
6.98877591532868));
#15486=CARTESIAN_POINT('Ctrl Pts',(-203.468597003262,-62.8298309839558,
7.04174535493012));
#15487=CARTESIAN_POINT('Ctrl Pts',(-204.330244780075,-62.4297360754195,
7.09471479453155));
#15488=CARTESIAN_POINT('Ctrl Pts',(-205.162571731653,-62.4835064634023,
7.14768423413298));
#15489=CARTESIAN_POINT('Ctrl Pts',(-205.99489868323,-62.537276851385,7.20065367373442));
#15490=CARTESIAN_POINT('Ctrl Pts',(-206.797904809573,-63.044912535887,7.25362311333586));
#15491=CARTESIAN_POINT('Ctrl Pts',(-207.203496589882,-63.773716156002,7.30659255293729));
#15492=CARTESIAN_POINT('Ctrl Pts',(-207.60908837019,-64.502519776117,7.35956199253873));
#15493=CARTESIAN_POINT('Ctrl Pts',(-207.617265804465,-65.4524913318451,
7.41253143214016));
#15494=CARTESIAN_POINT('Ctrl Pts',(-207.224280402533,-66.1881691708582,
7.46550087174159));
#15495=CARTESIAN_POINT('Ctrl Pts',(-206.831295000601,-66.9238470098713,
7.51847031134303));
#15496=CARTESIAN_POINT('Ctrl Pts',(-206.037146762462,-67.4452311321696,
7.57143975094447));
#15497=CARTESIAN_POINT('Ctrl Pts',(-205.205868802464,-67.5133219697927,
7.6244091905459));
#15498=CARTESIAN_POINT('Ctrl Pts',(-204.374590842466,-67.5814128074158,
7.67737863014734));
#15499=CARTESIAN_POINT('Ctrl Pts',(-203.506183160609,-67.1962103603639,
7.73034806974877));
#15500=CARTESIAN_POINT('Ctrl Pts',(-202.998718985249,-66.5342892777013,
7.78331750935021));
#15501=CARTESIAN_POINT('Ctrl Pts',(-202.666284477908,-66.1006716556147,
7.81801723873614));
#15502=CARTESIAN_POINT('Ctrl Pts',(-202.488746130884,-65.5483023359006,
7.85271696812208));
#15503=CARTESIAN_POINT('Ctrl Pts',(-202.484985611247,-64.9981409264881,
7.88741669750801));
#15504=CARTESIAN_POINT('Ctrl Pts',(-202.479185579191,-64.9986328469134,
7.61258330249198));
#15505=CARTESIAN_POINT('Ctrl Pts',(-202.484134115022,-65.7546174946183,
7.56461919626212));
#15506=CARTESIAN_POINT('Ctrl Pts',(-202.847051370263,-66.5147212446862,
7.51665509003227));
#15507=CARTESIAN_POINT('Ctrl Pts',(-203.440577913277,-66.9817598678951,
7.46869098380242));
#15508=CARTESIAN_POINT('Ctrl Pts',(-204.096042402105,-67.4975366870241,
7.41572154420098));
#15509=CARTESIAN_POINT('Ctrl Pts',(-205.032758385322,-67.655890760181,7.36275210459954));
#15510=CARTESIAN_POINT('Ctrl Pts',(-205.821340490962,-67.3842334651759,
7.30978266499811));
#15511=CARTESIAN_POINT('Ctrl Pts',(-206.609922596602,-67.1125761701709,
7.25681322539667));
#15512=CARTESIAN_POINT('Ctrl Pts',(-207.250370824665,-66.410907507004,7.20384378579524));
#15513=CARTESIAN_POINT('Ctrl Pts',(-207.449107286486,-65.600868469668,7.1508743461938));
#15514=CARTESIAN_POINT('Ctrl Pts',(-207.647843748306,-64.7908294323321,
7.09790490659237));
#15515=CARTESIAN_POINT('Ctrl Pts',(-207.404868443885,-63.8724200208271,
7.04493546699093));
#15516=CARTESIAN_POINT('Ctrl Pts',(-206.831559894925,-63.2666339769511,
6.99196602738949));
#15517=CARTESIAN_POINT('Ctrl Pts',(-206.258251345965,-62.660847933075,6.93899658778806));
#15518=CARTESIAN_POINT('Ctrl Pts',(-205.354609552468,-62.3676852568278,
6.88602714818662));
#15519=CARTESIAN_POINT('Ctrl Pts',(-204.534858862664,-62.5215300806918,
6.83305770858519));
#15520=CARTESIAN_POINT('Ctrl Pts',(-203.715108172859,-62.6753749045558,
6.78008826898375));
#15521=CARTESIAN_POINT('Ctrl Pts',(-202.979248586747,-63.276227228531,6.72711882938232));
#15522=CARTESIAN_POINT('Ctrl Pts',(-202.664594026326,-64.0486597051084,
6.67414938978088));
#15523=CARTESIAN_POINT('Ctrl Pts',(-202.542686940035,-64.3479243731608,
6.65362736068458));
#15524=CARTESIAN_POINT('Ctrl Pts',(-202.484004060027,-64.6729437646861,
6.63310533158828));
#15525=CARTESIAN_POINT('Ctrl Pts',(-202.485704986804,-64.9985525930702,
6.61258330249198));
#15526=CARTESIAN_POINT('Origin',(-205.,-65.,9.));
#15527=CARTESIAN_POINT('',(-202.484474743425,-65.0020481251356,5.61258330249198));
#15528=CARTESIAN_POINT('',(-202.478781684044,-65.0010375248543,5.88741669750801));
#15529=CARTESIAN_POINT('',(-202.4825,-65.,9.));
#15530=CARTESIAN_POINT('Ctrl Pts',(-202.478781684044,-65.0010375248543,
5.88741669750801));
#15531=CARTESIAN_POINT('Ctrl Pts',(-202.482826051254,-64.2242774991166,
5.93671979917295));
#15532=CARTESIAN_POINT('Ctrl Pts',(-202.869070789817,-63.4440435255548,
5.9860229008379));
#15533=CARTESIAN_POINT('Ctrl Pts',(-203.491087859415,-62.9795165331866,
6.03532600250284));
#15534=CARTESIAN_POINT('Ctrl Pts',(-204.159360128026,-62.4804458127945,
6.08829544210427));
#15535=CARTESIAN_POINT('Ctrl Pts',(-205.099774107373,-62.3457818808328,
6.14126488170571));
#15536=CARTESIAN_POINT('Ctrl Pts',(-205.881249284731,-62.6372539311573,
6.19423432130715));
#15537=CARTESIAN_POINT('Ctrl Pts',(-206.662724462089,-62.9287259814817,
6.24720376090858));
#15538=CARTESIAN_POINT('Ctrl Pts',(-207.285260837457,-63.6463340140924,
6.30017320051002));
#15539=CARTESIAN_POINT('Ctrl Pts',(-207.463491215347,-64.4611305171187,
6.35314264011145));
#15540=CARTESIAN_POINT('Ctrl Pts',(-207.641721593236,-65.2759270201451,
6.40611207971288));
#15541=CARTESIAN_POINT('Ctrl Pts',(-207.375645973648,-66.1879119935872,
6.45908151931432));
#15542=CARTESIAN_POINT('Ctrl Pts',(-206.787231933664,-66.7790366221529,
6.51205095891575));
#15543=CARTESIAN_POINT('Ctrl Pts',(-206.198817893681,-67.3701612507187,
6.56502039851719));
#15544=CARTESIAN_POINT('Ctrl Pts',(-205.288065433302,-67.640425534408,6.61798983811863));
#15545=CARTESIAN_POINT('Ctrl Pts',(-204.47245839072,-67.4659418359219,6.67095927772007));
#15546=CARTESIAN_POINT('Ctrl Pts',(-203.656851348138,-67.2914581374357,
6.7239287173215));
#15547=CARTESIAN_POINT('Ctrl Pts',(-202.936389723353,-66.6722264567739,
6.77689815692293));
#15548=CARTESIAN_POINT('Ctrl Pts',(-202.64132909894,-65.8920991358397,6.82986759652437));
#15549=CARTESIAN_POINT('Ctrl Pts',(-202.53447205207,-65.6095738010406,6.84905063018558));
#15550=CARTESIAN_POINT('Ctrl Pts',(-202.483408341005,-65.3059462486174,
6.8682336638468));
#15551=CARTESIAN_POINT('Ctrl Pts',(-202.485300085822,-65.0017052192927,
6.88741669750801));
#15552=CARTESIAN_POINT('Ctrl Pts',(-202.485704986804,-64.9985525930702,
6.61258330249198));
#15553=CARTESIAN_POINT('Ctrl Pts',(-202.488394324643,-65.5133731923927,
6.58013589198685));
#15554=CARTESIAN_POINT('Ctrl Pts',(-202.642036046849,-66.0296673142372,
6.54768848148171));
#15555=CARTESIAN_POINT('Ctrl Pts',(-202.935403284303,-66.4479674789478,
6.51524107097658));
#15556=CARTESIAN_POINT('Ctrl Pts',(-203.414316637431,-67.1308301470305,
6.46227163137514));
#15557=CARTESIAN_POINT('Ctrl Pts',(-204.265592878416,-67.5525428540164,
6.40930219177371));
#15558=CARTESIAN_POINT('Ctrl Pts',(-205.09901173566,-67.5197948517211,6.35633275217227));
#15559=CARTESIAN_POINT('Ctrl Pts',(-205.932430592905,-67.4870468494258,
6.30336331257083));
#15560=CARTESIAN_POINT('Ctrl Pts',(-206.747992066409,-66.9998381378491,
6.2503938729694));
#15561=CARTESIAN_POINT('Ctrl Pts',(-207.171847334398,-66.2815024676625,
6.19742443336796));
#15562=CARTESIAN_POINT('Ctrl Pts',(-207.595702602388,-65.5631667974759,
6.14445499376652));
#15563=CARTESIAN_POINT('Ctrl Pts',(-207.627851664864,-64.6137041686792,
6.09148555416509));
#15564=CARTESIAN_POINT('Ctrl Pts',(-207.253557571248,-63.8683429443391,
6.03851611456365));
#15565=CARTESIAN_POINT('Ctrl Pts',(-206.879263477633,-63.122981719999,5.98554667496222));
#15566=CARTESIAN_POINT('Ctrl Pts',(-206.098526227927,-62.5817219001155,
5.93257723536078));
#15567=CARTESIAN_POINT('Ctrl Pts',(-205.269231414325,-62.4926739613487,
5.87960779575935));
#15568=CARTESIAN_POINT('Ctrl Pts',(-204.439936600723,-62.4036260225818,
5.82663835615791));
#15569=CARTESIAN_POINT('Ctrl Pts',(-203.562084223227,-62.7667899649316,
5.77366891655648));
#15570=CARTESIAN_POINT('Ctrl Pts',(-203.038076905892,-63.4156934667291,
5.72069947695504));
#15571=CARTESIAN_POINT('Ctrl Pts',(-202.68155896544,-63.8571868053907,5.68466075213402));
#15572=CARTESIAN_POINT('Ctrl Pts',(-202.488836240528,-64.4309492584116,
5.648622027313));
#15573=CARTESIAN_POINT('Ctrl Pts',(-202.484474743425,-65.0020481251356,
5.61258330249198));
#15574=CARTESIAN_POINT('Origin',(-205.,-65.,9.));
#15575=CARTESIAN_POINT('',(-202.478344395066,-65.0004148924675,4.61258330249198));
#15576=CARTESIAN_POINT('',(-202.482172797578,-64.9977007737485,4.88741669750801));
#15577=CARTESIAN_POINT('',(-202.4825,-65.,9.));
#15578=CARTESIAN_POINT('Ctrl Pts',(-202.482172797578,-64.9977007737485,
4.88741669750801));
#15579=CARTESIAN_POINT('Ctrl Pts',(-202.480439688195,-64.8103463528036,
4.89926705529624));
#15580=CARTESIAN_POINT('Ctrl Pts',(-202.49957664238,-64.6233426993509,4.91111741308446));
#15581=CARTESIAN_POINT('Ctrl Pts',(-202.540911780016,-64.4413816920215,
4.92296777087269));
#15582=CARTESIAN_POINT('Ctrl Pts',(-202.725674056022,-63.6280414739628,
4.97593721047413));
#15583=CARTESIAN_POINT('Ctrl Pts',(-203.353948221845,-62.9154515500352,
5.02890665007556));
#15584=CARTESIAN_POINT('Ctrl Pts',(-204.137736910917,-62.6302591591322,
5.08187608967699));
#15585=CARTESIAN_POINT('Ctrl Pts',(-204.92152559999,-62.3450667682292,5.13484552927843));
#15586=CARTESIAN_POINT('Ctrl Pts',(-205.860828812312,-62.4872719103509,
5.18781496887987));
#15587=CARTESIAN_POINT('Ctrl Pts',(-206.525075204553,-62.9916885430472,
5.2407844084813));
#15588=CARTESIAN_POINT('Ctrl Pts',(-207.189321596795,-63.4961051757435,
5.29375384808274));
#15589=CARTESIAN_POINT('Ctrl Pts',(-207.578511168956,-64.3627332990145,
5.34672328768417));
#15590=CARTESIAN_POINT('Ctrl Pts',(-207.514241596105,-65.1943154242145,
5.39969272728561));
#15591=CARTESIAN_POINT('Ctrl Pts',(-207.449972023253,-66.0258975494145,
5.45266216688704));
#15592=CARTESIAN_POINT('Ctrl Pts',(-206.932243305388,-66.8224336765435,
5.50563160648848));
#15593=CARTESIAN_POINT('Ctrl Pts',(-206.198379393506,-67.2187960962853,
5.55860104608992));
#15594=CARTESIAN_POINT('Ctrl Pts',(-205.464515481624,-67.6151585160272,
5.61157048569135));
#15595=CARTESIAN_POINT('Ctrl Pts',(-204.514516375724,-67.6113472283819,
5.66453992529279));
#15596=CARTESIAN_POINT('Ctrl Pts',(-203.78385635698,-67.209109306307,5.71750936489422));
#15597=CARTESIAN_POINT('Ctrl Pts',(-203.053196338235,-66.8068713842322,
5.77047880449566));
#15598=CARTESIAN_POINT('Ctrl Pts',(-202.541875406646,-66.0062068277278,
5.82344824409709));
#15599=CARTESIAN_POINT('Ctrl Pts',(-202.484280219788,-65.1741357950644,
5.87641768369853));
#15600=CARTESIAN_POINT('Ctrl Pts',(-202.480293705675,-65.1165430847041,
5.88008402163502));
#15601=CARTESIAN_POINT('Ctrl Pts',(-202.478480931831,-65.0587999100541,
5.88375035957152));
#15602=CARTESIAN_POINT('Ctrl Pts',(-202.478781684044,-65.0010375248543,
5.88741669750801));
#15603=CARTESIAN_POINT('Ctrl Pts',(-202.484474743425,-65.0020481251356,
5.61258330249198));
#15604=CARTESIAN_POINT('Ctrl Pts',(-202.482425745747,-65.2703459650826,
5.59565258771156));
#15605=CARTESIAN_POINT('Ctrl Pts',(-202.521948972994,-65.5380559387795,
5.57872187293115));
#15606=CARTESIAN_POINT('Ctrl Pts',(-202.605591562129,-65.7911874943456,
5.56179115815073));
#15607=CARTESIAN_POINT('Ctrl Pts',(-202.867275792872,-66.5831349589198,
5.5088217185493));
#15608=CARTESIAN_POINT('Ctrl Pts',(-203.560806511531,-67.232386826823,5.45585227894786));
#15609=CARTESIAN_POINT('Ctrl Pts',(-204.368273112397,-67.4413296700853,
5.40288283934643));
#15610=CARTESIAN_POINT('Ctrl Pts',(-205.175739713264,-67.6502725133476,
5.34991339974499));
#15611=CARTESIAN_POINT('Ctrl Pts',(-206.097142196337,-67.4189063319689,
5.29694396014355));
#15612=CARTESIAN_POINT('Ctrl Pts',(-206.710114812539,-66.8532880905275,
5.24397452054212));
#15613=CARTESIAN_POINT('Ctrl Pts',(-207.323087428742,-66.2876698490862,
5.19100508094068));
#15614=CARTESIAN_POINT('Ctrl Pts',(-207.627630178073,-65.3877995475822,
5.13803564133925));
#15615=CARTESIAN_POINT('Ctrl Pts',(-207.484142366145,-64.5661727033922,
5.08506620173781));
#15616=CARTESIAN_POINT('Ctrl Pts',(-207.340654554217,-63.7445458592023,
5.03209676213638));
#15617=CARTESIAN_POINT('Ctrl Pts',(-206.74913618103,-63.0011624723264,4.97912732253494));
#15618=CARTESIAN_POINT('Ctrl Pts',(-205.980735963214,-62.6767853329884,
4.92615788293351));
#15619=CARTESIAN_POINT('Ctrl Pts',(-205.212335745398,-62.3524081936504,
4.87318844333207));
#15620=CARTESIAN_POINT('Ctrl Pts',(-204.267053682953,-62.4470373018503,
4.82021900373063));
#15621=CARTESIAN_POINT('Ctrl Pts',(-203.578201790692,-62.9172952032119,
4.7672495641292));
#15622=CARTESIAN_POINT('Ctrl Pts',(-202.907738797946,-63.3749995710904,
4.71569414358346));
#15623=CARTESIAN_POINT('Ctrl Pts',(-202.480197907909,-64.1885455944467,
4.66413872303772));
#15624=CARTESIAN_POINT('Ctrl Pts',(-202.478344395066,-65.0004148924675,
4.61258330249198));
#15625=CARTESIAN_POINT('Origin',(-205.,-65.,9.));
#15626=CARTESIAN_POINT('',(-202.483242763103,-64.9977147872857,3.61258330249198));
#15627=CARTESIAN_POINT('',(-202.486532876632,-65.000230478593,3.88741669750801));
#15628=CARTESIAN_POINT('',(-202.4825,-65.,9.));
#15629=CARTESIAN_POINT('Ctrl Pts',(-202.486532876632,-65.000230478593,3.88741669750801));
#15630=CARTESIAN_POINT('Ctrl Pts',(-202.48688726354,-64.5656588769883,3.91478375102096));
#15631=CARTESIAN_POINT('Ctrl Pts',(-202.593847112874,-64.1309238627515,
3.94215080453391));
#15632=CARTESIAN_POINT('Ctrl Pts',(-202.806413602928,-63.7560755624945,
3.96951785804685));
#15633=CARTESIAN_POINT('Ctrl Pts',(-203.217839986513,-63.0305497257151,
4.02248729764829));
#15634=CARTESIAN_POINT('Ctrl Pts',(-204.024893351068,-62.5293734155429,
4.07545673724972));
#15635=CARTESIAN_POINT('Ctrl Pts',(-204.857624944432,-62.482283051804,4.12842617685116));
#15636=CARTESIAN_POINT('Ctrl Pts',(-205.690356537796,-62.435192688065,4.18139561645259));
#15637=CARTESIAN_POINT('Ctrl Pts',(-206.548766359968,-62.8421882707593,
4.23436505605403));
#15638=CARTESIAN_POINT('Ctrl Pts',(-207.039364145592,-63.5167052992251,
4.28733449565546));
#15639=CARTESIAN_POINT('Ctrl Pts',(-207.529961931215,-64.1912223276909,
4.3403039352569));
#15640=CARTESIAN_POINT('Ctrl Pts',(-207.652747680291,-65.1332608019282,
4.39327337485833));
#15641=CARTESIAN_POINT('Ctrl Pts',(-207.351437091621,-65.9109955498349,
4.44624281445977));
#15642=CARTESIAN_POINT('Ctrl Pts',(-207.05012650295,-66.6887302977416,4.4992122540612));
#15643=CARTESIAN_POINT('Ctrl Pts',(-206.324719576535,-67.3021613193176,
4.55218169366264));
#15644=CARTESIAN_POINT('Ctrl Pts',(-205.50773879358,-67.4700952623667,4.60515113326408));
#15645=CARTESIAN_POINT('Ctrl Pts',(-204.690758010624,-67.6380292054158,
4.65812057286551));
#15646=CARTESIAN_POINT('Ctrl Pts',(-203.782203371129,-67.3604660699379,
4.71109001246695));
#15647=CARTESIAN_POINT('Ctrl Pts',(-203.198551244476,-66.764639246104,4.76405945206838));
#15648=CARTESIAN_POINT('Ctrl Pts',(-202.745474154612,-66.3021111903028,
4.80517853388159));
#15649=CARTESIAN_POINT('Ctrl Pts',(-202.488186444403,-65.6477943743447,
4.8462976156948));
#15650=CARTESIAN_POINT('Ctrl Pts',(-202.482172797578,-64.9977007737485,
4.88741669750801));
#15651=CARTESIAN_POINT('Ctrl Pts',(-202.478344395066,-65.0004148924675,
4.61258330249198));
#15652=CARTESIAN_POINT('Ctrl Pts',(-202.478293558463,-65.0226821661311,
4.61116928343628));
#15653=CARTESIAN_POINT('Ctrl Pts',(-202.478562944938,-65.0449481784791,
4.60975526438059));
#15654=CARTESIAN_POINT('Ctrl Pts',(-202.479156325318,-65.0672055531675,
4.60834124532489));
#15655=CARTESIAN_POINT('Ctrl Pts',(-202.501384474282,-65.9009713072382,
4.55537180572346));
#15656=CARTESIAN_POINT('Ctrl Pts',(-202.978262494288,-66.7226161208565,
4.50240236612202));
#15657=CARTESIAN_POINT('Ctrl Pts',(-203.691192165945,-67.1555026031265,
4.44943292652058));
#15658=CARTESIAN_POINT('Ctrl Pts',(-204.404121837602,-67.5883890853966,
4.39646348691915));
#15659=CARTESIAN_POINT('Ctrl Pts',(-205.353103160912,-67.6325172363185,
4.34349404731772));
#15660=CARTESIAN_POINT('Ctrl Pts',(-206.103128400557,-67.2676589581362,
4.29052460771628));
#15661=CARTESIAN_POINT('Ctrl Pts',(-206.853153640202,-66.9028006799539,
4.23755516811485));
#15662=CARTESIAN_POINT('Ctrl Pts',(-207.404222796182,-66.1289559726674,
4.18458572851341));
#15663=CARTESIAN_POINT('Ctrl Pts',(-207.50372884698,-65.3008509255024,4.13161628891197));
#15664=CARTESIAN_POINT('Ctrl Pts',(-207.603234897779,-64.4727458783375,
4.07864684931054));
#15665=CARTESIAN_POINT('Ctrl Pts',(-207.251177843396,-63.5903804912942,
4.02567740970911));
#15666=CARTESIAN_POINT('Ctrl Pts',(-206.608938670144,-63.0582261268744,
3.97270797010767));
#15667=CARTESIAN_POINT('Ctrl Pts',(-205.966699496891,-62.5260717624545,
3.91973853050623));
#15668=CARTESIAN_POINT('Ctrl Pts',(-205.034278204769,-62.3441284206583,
3.86676909090479));
#15669=CARTESIAN_POINT('Ctrl Pts',(-204.239091503311,-62.59579791241,3.81379965130336));
#15670=CARTESIAN_POINT('Ctrl Pts',(-203.443904801853,-62.8474674041617,
3.76083021170192));
#15671=CARTESIAN_POINT('Ctrl Pts',(-202.785952691059,-63.5327497294614,
3.70786077210049));
#15672=CARTESIAN_POINT('Ctrl Pts',(-202.566836741692,-64.3375153003988,
3.65489133249905));
#15673=CARTESIAN_POINT('Ctrl Pts',(-202.508498926336,-64.5517775000122,
3.64078865583003));
#15674=CARTESIAN_POINT('Ctrl Pts',(-202.481267868868,-64.7745092304446,
3.626685979161));
#15675=CARTESIAN_POINT('Ctrl Pts',(-202.483242763103,-64.9977147872857,
3.61258330249198));
#15676=CARTESIAN_POINT('Origin',(-205.,-65.,9.));
#15677=CARTESIAN_POINT('',(-202.486312984545,-65.0008035915154,2.61258330249198));
#15678=CARTESIAN_POINT('',(-202.481325023787,-65.002196172282,2.88741669750801));
#15679=CARTESIAN_POINT('',(-202.4825,-65.,9.));
#15680=CARTESIAN_POINT('Ctrl Pts',(-202.481325023787,-65.002196172282,2.88741669750801));
#15681=CARTESIAN_POINT('Ctrl Pts',(-202.487529219197,-64.3247893018804,
2.93030044674568));
#15682=CARTESIAN_POINT('Ctrl Pts',(-202.769932024913,-63.6428224125831,
2.97318419598334));
#15683=CARTESIAN_POINT('Ctrl Pts',(-203.258234470432,-63.1764260021977,
3.01606794522101));
#15684=CARTESIAN_POINT('Ctrl Pts',(-203.861379189701,-62.6003393276553,
3.06903738482244));
#15685=CARTESIAN_POINT('Ctrl Pts',(-204.778662179042,-62.3531455904109,
3.12200682442388));
#15686=CARTESIAN_POINT('Ctrl Pts',(-205.589606043438,-62.5481570193482,
3.17497626402531));
#15687=CARTESIAN_POINT('Ctrl Pts',(-206.400549907833,-62.7431684482854,
3.22794570362675));
#15688=CARTESIAN_POINT('Ctrl Pts',(-207.105154647285,-63.3803850434044,
3.28091514322819));
#15689=CARTESIAN_POINT('Ctrl Pts',(-207.380433386275,-64.1677102779642,
3.33388458282962));
#15690=CARTESIAN_POINT('Ctrl Pts',(-207.655712125266,-64.9550355125241,
3.38685402243106));
#15691=CARTESIAN_POINT('Ctrl Pts',(-207.501664863796,-65.8924693865247,
3.43982346203249));
#15692=CARTESIAN_POINT('Ctrl Pts',(-206.98890600592,-66.5502974511473,3.49279290163393));
#15693=CARTESIAN_POINT('Ctrl Pts',(-206.476147148043,-67.2081255157699,
3.54576234123536));
#15694=CARTESIAN_POINT('Ctrl Pts',(-205.60467669376,-67.5863477710145,3.5987317808368));
#15695=CARTESIAN_POINT('Ctrl Pts',(-204.773971829058,-67.5115892486015,
3.65170122043824));
#15696=CARTESIAN_POINT('Ctrl Pts',(-203.943266964357,-67.4368307261884,
3.70467066003967));
#15697=CARTESIAN_POINT('Ctrl Pts',(-203.153327689236,-66.9090914261176,
3.7576400996411));
#15698=CARTESIAN_POINT('Ctrl Pts',(-202.766257752983,-66.170284094389,3.81060953924254));
#15699=CARTESIAN_POINT('Ctrl Pts',(-202.57917036777,-65.8131870457086,3.83621192533103));
#15700=CARTESIAN_POINT('Ctrl Pts',(-202.486201341108,-65.4067802711058,
3.86181431141952));
#15701=CARTESIAN_POINT('Ctrl Pts',(-202.486532876632,-65.000230478593,3.88741669750801));
#15702=CARTESIAN_POINT('Ctrl Pts',(-202.483242763103,-64.9977147872857,
3.61258330249198));
#15703=CARTESIAN_POINT('Ctrl Pts',(-202.488685541649,-65.6128659154395,
3.57371653955957));
#15704=CARTESIAN_POINT('Ctrl Pts',(-202.715960735313,-66.2316159695124,
3.53484977662716));
#15705=CARTESIAN_POINT('Ctrl Pts',(-203.125278860397,-66.6865912568974,
3.49598301369474));
#15706=CARTESIAN_POINT('Ctrl Pts',(-203.683116716411,-67.3066528258837,
3.44301357409331));
#15707=CARTESIAN_POINT('Ctrl Pts',(-204.57907221638,-67.6225271472811,3.39004413449187));
#15708=CARTESIAN_POINT('Ctrl Pts',(-205.402444366375,-67.4894191989927,
3.33707469489044));
#15709=CARTESIAN_POINT('Ctrl Pts',(-206.225816516371,-67.3563112507042,
3.284105255289));
#15710=CARTESIAN_POINT('Ctrl Pts',(-206.976605316395,-66.7742210327298,
3.23113581568757));
#15711=CARTESIAN_POINT('Ctrl Pts',(-207.310653375596,-66.009975444743,3.17816637608613));
#15712=CARTESIAN_POINT('Ctrl Pts',(-207.644701434797,-65.2457298567563,
3.1251969364847));
#15713=CARTESIAN_POINT('Ctrl Pts',(-207.562008753175,-64.2993288987573,
3.07222749688326));
#15714=CARTESIAN_POINT('Ctrl Pts',(-207.100481195153,-63.6045974878118,
3.01925805728183));
#15715=CARTESIAN_POINT('Ctrl Pts',(-206.638953637131,-62.9098660768664,
2.96628861768039));
#15716=CARTESIAN_POINT('Ctrl Pts',(-205.798591202707,-62.4668042129746,
2.91331917807895));
#15717=CARTESIAN_POINT('Ctrl Pts',(-204.964611332898,-62.4785089645746,
2.86034973847752));
#15718=CARTESIAN_POINT('Ctrl Pts',(-204.130631463088,-62.4902137161746,
2.80738029887608));
#15719=CARTESIAN_POINT('Ctrl Pts',(-203.303034157892,-62.9566850832665,
2.75441085927465));
#15720=CARTESIAN_POINT('Ctrl Pts',(-202.861185402517,-63.6640952267508,
2.70144141967321));
#15721=CARTESIAN_POINT('Ctrl Pts',(-202.614113073159,-64.0596637778368,
2.67182204727947));
#15722=CARTESIAN_POINT('Ctrl Pts',(-202.487656834806,-64.5305692119616,
2.64220267488572));
#15723=CARTESIAN_POINT('Ctrl Pts',(-202.486312984545,-65.0008035915154,
2.61258330249198));
#15724=CARTESIAN_POINT('Origin',(-205.,-65.,9.));
#15725=CARTESIAN_POINT('',(-202.480291602729,-65.0019224916823,1.61258330249198));
#15726=CARTESIAN_POINT('',(-202.479332426993,-64.9985362476049,1.88741669750801));
#15727=CARTESIAN_POINT('',(-202.4825,-65.,9.));
#15728=CARTESIAN_POINT('Ctrl Pts',(-202.479332426993,-64.9985362476049,
1.88741669750801));
#15729=CARTESIAN_POINT('Ctrl Pts',(-202.478740698757,-64.9129225001756,
1.89284770286896));
#15730=CARTESIAN_POINT('Ctrl Pts',(-202.48272375902,-64.8273644585912,1.89827870822991));
#15731=CARTESIAN_POINT('Ctrl Pts',(-202.491463034604,-64.7422950299795,
1.90370971359086));
#15732=CARTESIAN_POINT('Ctrl Pts',(-202.576698547997,-63.9125996676488,
1.9566791531923));
#15733=CARTESIAN_POINT('Ctrl Pts',(-203.114364484717,-63.1293831459998,
2.00964859279373));
#15734=CARTESIAN_POINT('Ctrl Pts',(-203.857997602776,-62.7516673617973,
2.06261803239517));
#15735=CARTESIAN_POINT('Ctrl Pts',(-204.601630720835,-62.3739515775949,
2.1155874719966));
#15736=CARTESIAN_POINT('Ctrl Pts',(-205.551231020233,-62.401736530839,2.16855691159804));
#15737=CARTESIAN_POINT('Ctrl Pts',(-206.271507118528,-62.8222858415902,
2.22152635119947));
#15738=CARTESIAN_POINT('Ctrl Pts',(-206.991783216823,-63.2428351523415,
2.27449579080091));
#15739=CARTESIAN_POINT('Ctrl Pts',(-207.482735114015,-64.0561488205997,
2.32746523040235));
#15740=CARTESIAN_POINT('Ctrl Pts',(-207.519313161291,-64.8894083635227,
2.38043467000378));
#15741=CARTESIAN_POINT('Ctrl Pts',(-207.555891208567,-65.7226679064456,
2.43340410960522));
#15742=CARTESIAN_POINT('Ctrl Pts',(-207.138095405927,-66.5758733240332,
2.48637354920665));
#15743=CARTESIAN_POINT('Ctrl Pts',(-206.457441035269,-67.057920041525,2.53934298880809));
#15744=CARTESIAN_POINT('Ctrl Pts',(-205.776786664612,-67.5399667590167,
2.59231242840953));
#15745=CARTESIAN_POINT('Ctrl Pts',(-204.833273725938,-67.6508547764125,
2.64528186801096));
#15746=CARTESIAN_POINT('Ctrl Pts',(-204.059403267518,-67.3397536362125,
2.6982513076124));
#15747=CARTESIAN_POINT('Ctrl Pts',(-203.285532809097,-67.0286524960126,
2.75122074721383));
#15748=CARTESIAN_POINT('Ctrl Pts',(-202.681304830931,-66.2955621982167,
2.80419018681527));
#15749=CARTESIAN_POINT('Ctrl Pts',(-202.523694066448,-65.4765272433986,
2.8571596264167));
#15750=CARTESIAN_POINT('Ctrl Pts',(-202.49368405727,-65.3205782091337,2.86724531678047));
#15751=CARTESIAN_POINT('Ctrl Pts',(-202.479865879124,-65.1615133044501,
2.87733100714424));
#15752=CARTESIAN_POINT('Ctrl Pts',(-202.481325023787,-65.002196172282,2.88741669750801));
#15753=CARTESIAN_POINT('Ctrl Pts',(-202.486312984545,-65.0008035915154,
2.61258330249198));
#15754=CARTESIAN_POINT('Ctrl Pts',(-202.485253576752,-65.3715070696305,
2.58923323528429));
#15755=CARTESIAN_POINT('Ctrl Pts',(-202.561948551986,-65.7417935032391,
2.5658831680766));
#15756=CARTESIAN_POINT('Ctrl Pts',(-202.718600795358,-66.0744240820748,
2.54253310086891));
#15757=CARTESIAN_POINT('Ctrl Pts',(-203.073965149126,-66.8289938740376,
2.48956366126747));
#15758=CARTESIAN_POINT('Ctrl Pts',(-203.840794062215,-67.3897845380866,
2.43659422166603));
#15759=CARTESIAN_POINT('Ctrl Pts',(-204.667577469299,-67.4997328895863,
2.3836247820646));
#15760=CARTESIAN_POINT('Ctrl Pts',(-205.494360876384,-67.6096812410859,
2.33065534246316));
#15761=CARTESIAN_POINT('Ctrl Pts',(-206.381098777463,-67.2687872800362,
2.27768590286173));
#15762=CARTESIAN_POINT('Ctrl Pts',(-206.92131542659,-66.6333146422909,2.22471646326029));
#15763=CARTESIAN_POINT('Ctrl Pts',(-207.461532075717,-65.9978420045456,
2.17174702365886));
#15764=CARTESIAN_POINT('Ctrl Pts',(-207.655227472892,-65.0677906901045,
2.11877758405742));
#15765=CARTESIAN_POINT('Ctrl Pts',(-207.413612828359,-64.2694915404195,
2.06580814445599));
#15766=CARTESIAN_POINT('Ctrl Pts',(-207.171998183825,-63.4711923907344,
2.01283870485455));
#15767=CARTESIAN_POINT('Ctrl Pts',(-206.495073497584,-62.8046454058054,
1.95986926525311));
#15768=CARTESIAN_POINT('Ctrl Pts',(-205.693137061413,-62.5753909354637,
1.90689982565168));
#15769=CARTESIAN_POINT('Ctrl Pts',(-204.891200625243,-62.346136465122,1.85393038605024));
#15770=CARTESIAN_POINT('Ctrl Pts',(-203.964252439144,-62.5541745093678,
1.80096094644881));
#15771=CARTESIAN_POINT('Ctrl Pts',(-203.337200786238,-63.104143779992,1.74799150684737));
#15772=CARTESIAN_POINT('Ctrl Pts',(-202.802880500195,-63.572780991349,1.70285543872891));
#15773=CARTESIAN_POINT('Ctrl Pts',(-202.486315214849,-64.289694612059,1.65771937061044));
#15774=CARTESIAN_POINT('Ctrl Pts',(-202.480291602729,-65.0019224916823,
1.61258330249198));
#15775=CARTESIAN_POINT('Origin',(-205.,-65.,9.));
#15776=CARTESIAN_POINT('',(-202.480232352617,-64.9981364767374,0.612583302491977));
#15777=CARTESIAN_POINT('',(-202.485823045017,-64.9986459985219,0.88741669750801));
#15778=CARTESIAN_POINT('',(-202.4825,-65.,9.));
#15779=CARTESIAN_POINT('',(-206.913465996665,-63.364012796625,0.));
#15780=CARTESIAN_POINT('Ctrl Pts',(-202.480232352617,-64.9981364767374,
0.612583302491977));
#15781=CARTESIAN_POINT('Ctrl Pts',(-202.486197484929,-65.7125427933529,
0.567297187132291));
#15782=CARTESIAN_POINT('Ctrl Pts',(-202.805075366122,-66.4315079379949,
0.522011071772604));
#15783=CARTESIAN_POINT('Ctrl Pts',(-203.342531992607,-66.9003622927727,
0.476724956412918));
#15784=CARTESIAN_POINT('Ctrl Pts',(-203.971174482448,-67.4487633254074,
0.423755516811482));
#15785=CARTESIAN_POINT('Ctrl Pts',(-204.898856465583,-67.6549855987664,
0.370786077210047));
#15786=CARTESIAN_POINT('Ctrl Pts',(-205.700051222351,-67.4230386418016,
0.317816637608611));
#15787=CARTESIAN_POINT('Ctrl Pts',(-206.501245979118,-67.1910916848368,
0.264847198007176));
#15788=CARTESIAN_POINT('Ctrl Pts',(-207.175953509519,-66.5209754975483,
0.21187775840574));
#15789=CARTESIAN_POINT('Ctrl Pts',(-207.415129522268,-65.7234141851915,
0.158908318804305));
#15790=CARTESIAN_POINT('Ctrl Pts',(-207.654305535017,-64.9258528728346,
0.10593887920287));
#15791=CARTESIAN_POINT('Ctrl Pts',(-207.457950030113,-64.0008464354095,
0.0529694396014348));
#15792=CARTESIAN_POINT('Ctrl Pts',(-206.913465996665,-63.364012796625,-2.46594462980148E-16));
#15793=CARTESIAN_POINT('',(-203.082854832445,-63.3612166619665,8.28281533331144E-15));
#15794=CARTESIAN_POINT('Origin',(-205.,-65.,0.));
#15795=CARTESIAN_POINT('Ctrl Pts',(-203.082851793447,-63.3612143523572,
5.48172618408671E-15));
#15796=CARTESIAN_POINT('Ctrl Pts',(-203.614822557714,-62.7406365668551,
0.0519060689144995));
#15797=CARTESIAN_POINT('Ctrl Pts',(-204.477412283426,-62.4011241208618,
0.103812137828994));
#15798=CARTESIAN_POINT('Ctrl Pts',(-205.289478531141,-62.4950491013773,
0.155718206743488));
#15799=CARTESIAN_POINT('Ctrl Pts',(-206.118181127201,-62.5908982705888,
0.208687646344923));
#15800=CARTESIAN_POINT('Ctrl Pts',(-206.894268948213,-63.1381259592108,
0.261657085946359));
#15801=CARTESIAN_POINT('Ctrl Pts',(-207.262498103941,-63.8863946495074,
0.314626525547794));
#15802=CARTESIAN_POINT('Ctrl Pts',(-207.630727259668,-64.634663339804,0.367595965149229));
#15803=CARTESIAN_POINT('Ctrl Pts',(-207.591097750112,-65.5839730317752,
0.420565404750665));
#15804=CARTESIAN_POINT('Ctrl Pts',(-207.161527602495,-66.298919576317,0.473534844352101));
#15805=CARTESIAN_POINT('Ctrl Pts',(-206.731957454879,-67.0138661208588,
0.526504283953536));
#15806=CARTESIAN_POINT('Ctrl Pts',(-205.912446669203,-67.4944495179713,
0.579473723554972));
#15807=CARTESIAN_POINT('Ctrl Pts',(-205.078774820569,-67.520492478951,0.632443163156408));
#15808=CARTESIAN_POINT('Ctrl Pts',(-204.245102971934,-67.5465354399307,
0.685412602757844));
#15809=CARTESIAN_POINT('Ctrl Pts',(-203.39727006034,-67.1180379647775,0.738382042359279));
#15810=CARTESIAN_POINT('Ctrl Pts',(-202.923859465156,-66.4313628808451,
0.791351481960714));
#15811=CARTESIAN_POINT('Ctrl Pts',(-202.637667457015,-66.0162455953229,
0.823373220476479));
#15812=CARTESIAN_POINT('Ctrl Pts',(-202.488311578843,-65.5067748931336,
0.855394958992245));
#15813=CARTESIAN_POINT('Ctrl Pts',(-202.485823045017,-64.9986459985219,
0.88741669750801));
#15814=CARTESIAN_POINT('Origin',(-205.,-65.,-2.20842344717744));
#15815=CARTESIAN_POINT('',(-201.92132715551,-64.9999599234514,16.2084234471775));
#15816=CARTESIAN_POINT('',(-201.931378654624,-64.9992193623962,16.2915765528226));
#15817=CARTESIAN_POINT('',(-201.9265,-64.9999999999997,-2.20842344717744));
#15818=CARTESIAN_POINT('',(-205.793799282533,-67.9692229537457,17.));
#15819=CARTESIAN_POINT('Ctrl Pts',(-201.931378654624,-64.9992193623962,
16.2915765528226));
#15820=CARTESIAN_POINT('Ctrl Pts',(-201.930449249078,-64.5288570727101,
16.315839943476));
#15821=CARTESIAN_POINT('Ctrl Pts',(-202.253363122225,-63.0329492967313,
16.3930727737308));
#15822=CARTESIAN_POINT('Ctrl Pts',(-204.58235400734,-61.3907532347673,16.5232750435871));
#15823=CARTESIAN_POINT('Ctrl Pts',(-207.810233625888,-62.6929017394991,
16.6821833623914));
#15824=CARTESIAN_POINT('Ctrl Pts',(-208.45647866392,-66.1152964431386,16.8410916811957));
#15825=CARTESIAN_POINT('Ctrl Pts',(-206.782006578242,-67.7050332130129,
16.9470305603986));
#15826=CARTESIAN_POINT('Ctrl Pts',(-205.793799282533,-67.9692229537457,
17.));
#15827=CARTESIAN_POINT('',(-204.206200717467,-67.9692229537457,17.));
#15828=CARTESIAN_POINT('Origin',(-205.,-65.,17.));
#15829=CARTESIAN_POINT('Ctrl Pts',(-201.92132715551,-64.9999599234514,16.2084234471775));
#15830=CARTESIAN_POINT('Ctrl Pts',(-201.921326964282,-64.9985177121332,
16.2084984707981));
#15831=CARTESIAN_POINT('Ctrl Pts',(-201.921978795173,-63.9788214197569,
16.2615429340201));
#15832=CARTESIAN_POINT('Ctrl Pts',(-203.036142175806,-61.9425259545107,
16.3675568368436));
#15833=CARTESIAN_POINT('Ctrl Pts',(-206.506723058425,-61.6929032655643,
16.5264651556479));
#15834=CARTESIAN_POINT('Ctrl Pts',(-208.5958014629,-64.4760115385876,16.6853734744522));
#15835=CARTESIAN_POINT('Ctrl Pts',(-207.396688180815,-67.7159880867316,
16.8432184225696));
#15836=CARTESIAN_POINT('Ctrl Pts',(-205.168807240445,-68.2310729455545,
16.9480939310855));
#15837=CARTESIAN_POINT('Ctrl Pts',(-204.204431258832,-67.9745848956374,
17.));
#15838=CARTESIAN_POINT('Origin',(-205.,-65.,-2.20842344717744));
#15839=CARTESIAN_POINT('',(-201.928225509175,-64.9973269163706,15.2084234471775));
#15840=CARTESIAN_POINT('',(-201.926883815323,-65.0028204616814,15.2915765528226));
#15841=CARTESIAN_POINT('',(-201.9265,-64.9999999999997,-2.20842344717744));
#15842=CARTESIAN_POINT('Ctrl Pts',(-201.926883815323,-65.0028204616813,
15.2915765528226));
#15843=CARTESIAN_POINT('Ctrl Pts',(-201.933858564409,-64.2344951248146,
15.3313566392007));
#15844=CARTESIAN_POINT('Ctrl Pts',(-202.61466622664,-62.4320797304894,15.4241061651802));
#15845=CARTESIAN_POINT('Ctrl Pts',(-205.641600447141,-61.4231649792265,
15.5698251307612));
#15846=CARTESIAN_POINT('Ctrl Pts',(-208.354330260832,-63.6021006605898,
15.7287334495655));
#15847=CARTESIAN_POINT('Ctrl Pts',(-207.991779545523,-67.0626823173804,
15.8876417683699));
#15848=CARTESIAN_POINT('Ctrl Pts',(-204.886538848565,-68.6320809475727,
16.0465500871742));
#15849=CARTESIAN_POINT('Ctrl Pts',(-202.343324085074,-67.1406706620033,
16.1811950153251));
#15850=CARTESIAN_POINT('Ctrl Pts',(-201.93247823553,-65.5557055973133,16.2628705038745));
#15851=CARTESIAN_POINT('Ctrl Pts',(-201.931378654624,-64.9992193623962,
16.2915765528226));
#15852=CARTESIAN_POINT('Ctrl Pts',(-201.928225509175,-64.9973269163706,
15.2084234471775));
#15853=CARTESIAN_POINT('Ctrl Pts',(-201.925723596777,-64.6958495188348,
15.2240151665228));
#15854=CARTESIAN_POINT('Ctrl Pts',(-202.105046180913,-63.3730808756464,
15.2925763254695));
#15855=CARTESIAN_POINT('Ctrl Pts',(-204.001159743508,-61.5060359832025,
15.4141069240177));
#15856=CARTESIAN_POINT('Ctrl Pts',(-207.396164971614,-62.2679882236812,
15.5730152428221));
#15857=CARTESIAN_POINT('Ctrl Pts',(-208.594390890487,-65.5346291179969,
15.7319235616264));
#15858=CARTESIAN_POINT('Ctrl Pts',(-206.497323624104,-68.3111057941983,
15.8908318804307));
#15859=CARTESIAN_POINT('Ctrl Pts',(-203.02915628941,-68.0521657341669,16.0496651756144));
#15860=CARTESIAN_POINT('Ctrl Pts',(-201.921461978279,-66.0167720257951,
16.1555290311966));
#15861=CARTESIAN_POINT('Ctrl Pts',(-201.92132715551,-64.9999599234514,16.2084234471775));
#15862=CARTESIAN_POINT('Origin',(-205.,-65.,-2.20842344717744));
#15863=CARTESIAN_POINT('',(-201.930817979872,-65.0014123516849,14.2084234471775));
#15864=CARTESIAN_POINT('',(-201.921592942543,-64.9991754636855,14.2915765528226));
#15865=CARTESIAN_POINT('',(-201.9265,-64.9999999999997,-2.20842344717744));
#15866=CARTESIAN_POINT('Ctrl Pts',(-201.921592942543,-64.9991754636855,
14.2915765528226));
#15867=CARTESIAN_POINT('Ctrl Pts',(-201.92143307583,-64.9544248847186,14.293903895324));
#15868=CARTESIAN_POINT('Ctrl Pts',(-201.942607559848,-63.8913226189859,
14.3492006774268));
#15869=CARTESIAN_POINT('Ctrl Pts',(-203.167704028449,-61.8618209334909,
14.4574668991311));
#15870=CARTESIAN_POINT('Ctrl Pts',(-206.64567409827,-61.7600568166538,14.6163752179354));
#15871=CARTESIAN_POINT('Ctrl Pts',(-208.614908982248,-64.6286359675596,
14.7752835367397));
#15872=CARTESIAN_POINT('Ctrl Pts',(-207.270034820723,-67.8376783991727,
14.934191855544));
#15873=CARTESIAN_POINT('Ctrl Pts',(-203.844019947069,-68.4451671656806,
15.0931001743483));
#15874=CARTESIAN_POINT('Ctrl Pts',(-202.070137442914,-66.5327694250874,
15.2122284067745));
#15875=CARTESIAN_POINT('Ctrl Pts',(-201.924571290698,-65.2575638567064,
15.2783871995992));
#15876=CARTESIAN_POINT('Ctrl Pts',(-201.926883815323,-65.0028204616813,
15.2915765528226));
#15877=CARTESIAN_POINT('Ctrl Pts',(-201.930817979872,-65.0014123516849,
14.2084234471775));
#15878=CARTESIAN_POINT('Ctrl Pts',(-201.933314343602,-64.3986294258202,
14.2395318622475));
#15879=CARTESIAN_POINT('Ctrl Pts',(-202.39654106013,-62.7659248440265,14.323609716919));
#15880=CARTESIAN_POINT('Ctrl Pts',(-205.050996575713,-61.3664239142234,
14.4606570111919));
#15881=CARTESIAN_POINT('Ctrl Pts',(-208.082123040074,-63.0749042303987,
14.6195653299962));
#15882=CARTESIAN_POINT('Ctrl Pts',(-208.287593522688,-66.548290973518,14.7784736488005));
#15883=CARTESIAN_POINT('Ctrl Pts',(-205.479035063749,-68.6022215651833,
14.9373819676048));
#15884=CARTESIAN_POINT('Ctrl Pts',(-202.549962560241,-67.4761806836253,
15.0806985670638));
#15885=CARTESIAN_POINT('Ctrl Pts',(-201.934223294258,-65.7200527158195,
15.1710457269214));
#15886=CARTESIAN_POINT('Ctrl Pts',(-201.928225509175,-64.9973269163706,
15.2084234471775));
#15887=CARTESIAN_POINT('Origin',(-205.,-65.,-2.20842344717744));
#15888=CARTESIAN_POINT('',(-201.923048984138,-65.0020215843026,13.2084234471775));
#15889=CARTESIAN_POINT('',(-201.929343708848,-64.9976509895539,13.2915765528226));
#15890=CARTESIAN_POINT('',(-201.9265,-64.9999999999997,-2.20842344717744));
#15891=CARTESIAN_POINT('Ctrl Pts',(-201.929343708848,-64.9976509895539,
13.2915765528225));
#15892=CARTESIAN_POINT('Ctrl Pts',(-201.926890311751,-64.6523061159044,
13.3094205910487));
#15893=CARTESIAN_POINT('Ctrl Pts',(-202.14012767651,-63.2847573174409,13.3802340688762));
#15894=CARTESIAN_POINT('Ctrl Pts',(-204.150352533451,-61.4667896441583,
13.5040169863052));
#15895=CARTESIAN_POINT('Ctrl Pts',(-207.509958448151,-62.3721520583455,
13.6629253051096));
#15896=CARTESIAN_POINT('Ctrl Pts',(-208.568462516575,-65.6866960888727,
13.8218336239139));
#15897=CARTESIAN_POINT('Ctrl Pts',(-206.355440022032,-68.371684831825,13.9807419427182));
#15898=CARTESIAN_POINT('Ctrl Pts',(-202.950376476172,-67.9714987504005,
14.1373229190211));
#15899=CARTESIAN_POINT('Ctrl Pts',(-201.925071582081,-65.9729312232913,
14.2409344557225));
#15900=CARTESIAN_POINT('Ctrl Pts',(-201.921592942543,-64.9991754636855,
14.2915765528226));
#15901=CARTESIAN_POINT('Ctrl Pts',(-201.923048984138,-65.0020215843026,
13.2084234471775));
#15902=CARTESIAN_POINT('Ctrl Pts',(-201.92987213238,-64.1043840848538,13.2550485579722));
#15903=CARTESIAN_POINT('Ctrl Pts',(-202.817794830182,-62.1752162381125,
13.3546431083684));
#15904=CARTESIAN_POINT('Ctrl Pts',(-206.096501589105,-61.5354422759257,
13.5072070983661));
#15905=CARTESIAN_POINT('Ctrl Pts',(-208.506292006242,-64.0453312989241,
13.6661154171704));
#15906=CARTESIAN_POINT('Ctrl Pts',(-207.701553100804,-67.4304499187966,
13.8250237359747));
#15907=CARTESIAN_POINT('Ctrl Pts',(-204.420060507976,-68.5873592139186,
13.983932054779));
#15908=CARTESIAN_POINT('Ctrl Pts',(-202.208561914266,-66.8727735695644,
14.1117319585133));
#15909=CARTESIAN_POINT('Ctrl Pts',(-201.929063693496,-65.4250100277401,
14.1865624226461));
#15910=CARTESIAN_POINT('Ctrl Pts',(-201.930817979872,-65.0014123516849,
14.2084234471775));
#15911=CARTESIAN_POINT('Origin',(-205.,-65.,-2.20842344717744));
#15912=CARTESIAN_POINT('',(-201.924541298626,-64.9974318278238,12.2084234471775));
#15913=CARTESIAN_POINT('',(-201.930084794051,-65.0019865735648,12.2915765528226));
#15914=CARTESIAN_POINT('',(-201.9265,-64.9999999999997,-2.20842344717744));
#15915=CARTESIAN_POINT('Ctrl Pts',(-201.930084794051,-65.0019865735648,
12.2915765528226));
#15916=CARTESIAN_POINT('Ctrl Pts',(-201.933904603767,-64.3559473602958,
12.3249372867734));
#15917=CARTESIAN_POINT('Ctrl Pts',(-202.449144797282,-62.6785687029257,
12.4112674603257));
#15918=CARTESIAN_POINT('Ctrl Pts',(-205.205168530226,-61.3718624466171,
12.5505670734794));
#15919=CARTESIAN_POINT('Ctrl Pts',(-208.161051598535,-63.2074518072919,
12.7094753922837));
#15920=CARTESIAN_POINT('Ctrl Pts',(-208.218917891802,-66.6864293160267,
12.868383711088));
#15921=CARTESIAN_POINT('Ctrl Pts',(-205.32571623889,-68.6193072768529,13.0272920298923));
#15922=CARTESIAN_POINT('Ctrl Pts',(-202.492314928424,-67.3895978490803,
13.1683563104705));
#15923=CARTESIAN_POINT('Ctrl Pts',(-201.934173140205,-65.6774509959268,
13.2564511514472));
#15924=CARTESIAN_POINT('Ctrl Pts',(-201.929343708848,-64.9976509895539,
13.2915765528225));
#15925=CARTESIAN_POINT('Ctrl Pts',(-201.924541298626,-64.9974318278238,
12.2084234471775));
#15926=CARTESIAN_POINT('Ctrl Pts',(-201.9229576152,-64.8206202024618,12.2175958140955));
#15927=CARTESIAN_POINT('Ctrl Pts',(-202.017351259948,-63.6244303792901,
12.279737620615));
#15928=CARTESIAN_POINT('Ctrl Pts',(-203.586717658077,-61.6521486021326,
12.3948488667359));
#15929=CARTESIAN_POINT('Ctrl Pts',(-207.048871845595,-61.9987335805548,
12.5537571855402));
#15930=CARTESIAN_POINT('Ctrl Pts',(-208.632643224891,-65.0968460677781,
12.7126655043445));
#15931=CARTESIAN_POINT('Ctrl Pts',(-206.886047896905,-68.1061711625154,
12.8715738231488));
#15932=CARTESIAN_POINT('Ctrl Pts',(-203.410344937013,-68.2677932524411,
13.0304821419532));
#15933=CARTESIAN_POINT('Ctrl Pts',(-201.984214425865,-66.265134355684,13.1427653499627));
#15934=CARTESIAN_POINT('Ctrl Pts',(-201.922120551042,-65.1241640810951,
13.2020791183708));
#15935=CARTESIAN_POINT('Ctrl Pts',(-201.923048984138,-65.0020215843026,
13.2084234471775));
#15936=CARTESIAN_POINT('Origin',(-205.,-65.,-2.20842344717744));
#15937=CARTESIAN_POINT('',(-201.931350607177,-64.9994302461114,11.2084234471775));
#15938=CARTESIAN_POINT('',(-201.922104720032,-65.0013994359743,11.2915765528226));
#15939=CARTESIAN_POINT('',(-201.9265,-64.9999999999997,-2.20842344717744));
#15940=CARTESIAN_POINT('Ctrl Pts',(-201.922104720032,-65.0013994359743,
11.2915765528226));
#15941=CARTESIAN_POINT('Ctrl Pts',(-201.927430148624,-64.0611595253334,
11.3404539824981));
#15942=CARTESIAN_POINT('Ctrl Pts',(-202.890890769671,-62.0925255947041,
11.4423008517751));
#15943=CARTESIAN_POINT('Ctrl Pts',(-206.242557904149,-61.585102331427,11.5971171606536));
#15944=CARTESIAN_POINT('Ctrl Pts',(-208.543651054332,-64.1950071819504,
11.7560254794579));
#15945=CARTESIAN_POINT('Ctrl Pts',(-207.59596452456,-67.5429204508222,11.9149337982622));
#15946=CARTESIAN_POINT('Ctrl Pts',(-204.268326733228,-68.5595126720785,
12.0738421170665));
#15947=CARTESIAN_POINT('Ctrl Pts',(-202.169249466841,-66.7844550251247,
12.1993897019199));
#15948=CARTESIAN_POINT('Ctrl Pts',(-201.927839593915,-65.3817142135618,
12.271967847172));
#15949=CARTESIAN_POINT('Ctrl Pts',(-201.930084794051,-65.0019865735648,
12.2915765528226));
#15950=CARTESIAN_POINT('Ctrl Pts',(-201.931350607177,-64.9994302461114,
11.2084234471775));
#15951=CARTESIAN_POINT('Ctrl Pts',(-201.930559226518,-64.5208267214804,
11.2331125098202));
#15952=CARTESIAN_POINT('Ctrl Pts',(-202.261422759148,-63.0164333097365,
11.3107710120644));
#15953=CARTESIAN_POINT('Ctrl Pts',(-204.612026051834,-61.3868362650263,
11.4413989539101));
#15954=CARTESIAN_POINT('Ctrl Pts',(-207.82721483571,-62.7169467301605,11.6003072727144));
#15955=CARTESIAN_POINT('Ctrl Pts',(-208.450444657403,-66.140134915869,11.7592155915187));
#15956=CARTESIAN_POINT('Ctrl Pts',(-205.910345382095,-68.5180601537614,
11.918123910323));
#15957=CARTESIAN_POINT('Ctrl Pts',(-202.730442754502,-67.7195796399602,
12.0678598622093));
#15958=CARTESIAN_POINT('Ctrl Pts',(-201.932103217895,-65.8416884604287,
12.1646263744941));
#15959=CARTESIAN_POINT('Ctrl Pts',(-201.924541298626,-64.9974318278238,
12.2084234471775));
#15960=CARTESIAN_POINT('Origin',(-205.,-65.,-2.20842344717744));
#15961=CARTESIAN_POINT('',(-201.926636231845,-65.0028238856699,10.2084234471775));
#15962=CARTESIAN_POINT('',(-201.925849867817,-64.9972120766658,10.2915765528225));
#15963=CARTESIAN_POINT('',(-201.9265,-64.9999999999997,-2.20842344717744));
#15964=CARTESIAN_POINT('Ctrl Pts',(-201.925849867817,-64.9972120766658,
10.2915765528225));
#15965=CARTESIAN_POINT('Ctrl Pts',(-201.923807687974,-64.7767419557002,
10.3030012386214));
#15966=CARTESIAN_POINT('Ctrl Pts',(-202.04610426792,-63.5363314374797,10.3673953640217));
#15967=CARTESIAN_POINT('Ctrl Pts',(-203.73008217778,-61.5951820963824,10.4847589290234));
#15968=CARTESIAN_POINT('Ctrl Pts',(-207.17440677989,-62.0883971102576,10.6436672478277));
#15969=CARTESIAN_POINT('Ctrl Pts',(-208.625259549091,-65.2509371110651,
10.802575566632));
#15970=CARTESIAN_POINT('Ctrl Pts',(-206.752514882462,-68.1834207731203,
10.9614838854363));
#15971=CARTESIAN_POINT('Ctrl Pts',(-203.273084159089,-68.1973798508147,
11.1203922042406));
#15972=CARTESIAN_POINT('Ctrl Pts',(-201.960112831003,-66.1773468477829,
11.2304230933694));
#15973=CARTESIAN_POINT('Ctrl Pts',(-201.921658876075,-65.0801161580395,
11.2874845428967));
#15974=CARTESIAN_POINT('Ctrl Pts',(-201.922104720032,-65.0013994359743,
11.2915765528226));
#15975=CARTESIAN_POINT('Ctrl Pts',(-201.926636231845,-65.0028238856699,
10.2084234471775));
#15976=CARTESIAN_POINT('Ctrl Pts',(-201.933742916194,-64.2264373124871,
10.248629205545));
#15977=CARTESIAN_POINT('Ctrl Pts',(-202.62647814666,-62.4159028227408,10.3418044035139));
#15978=CARTESIAN_POINT('Ctrl Pts',(-205.670288212686,-61.4284191634349,
10.4879490410842));
#15979=CARTESIAN_POINT('Ctrl Pts',(-208.365419590609,-63.6290780695714,
10.6468573598886));
#15980=CARTESIAN_POINT('Ctrl Pts',(-207.975171902461,-67.0865828790137,
10.8057656786928));
#15981=CARTESIAN_POINT('Ctrl Pts',(-204.857319867018,-68.6311318262819,
10.9646739974972));
#15982=CARTESIAN_POINT('Ctrl Pts',(-202.334362656145,-67.1239410478955,
11.0988932536587));
#15983=CARTESIAN_POINT('Ctrl Pts',(-201.932257103454,-65.5476522781161,
11.1801430702188));
#15984=CARTESIAN_POINT('Ctrl Pts',(-201.931350607177,-64.9994302461114,
11.2084234471775));
#15985=CARTESIAN_POINT('Origin',(-205.,-65.,-2.20842344717744));
#15986=CARTESIAN_POINT('',(-201.921694744017,-64.9990313139748,9.20842344717746));
#15987=CARTESIAN_POINT('',(-201.931440561712,-65.000145803285,9.29157655282255));
#15988=CARTESIAN_POINT('',(-201.9265,-64.9999999999997,-2.20842344717744));
#15989=CARTESIAN_POINT('Ctrl Pts',(-201.931440561712,-65.000145803285,9.29157655282255));
#15990=CARTESIAN_POINT('Ctrl Pts',(-201.931661195711,-64.4778423231913,
9.31851793434612));
#15991=CARTESIAN_POINT('Ctrl Pts',(-202.306392174211,-62.9283411178457,
9.39842875547113));
#15992=CARTESIAN_POINT('Ctrl Pts',(-204.76572719775,-61.3736254349403,9.53130901619758));
#15993=CARTESIAN_POINT('Ctrl Pts',(-207.921565691441,-62.8389978846421,
9.69021733500189));
#15994=CARTESIAN_POINT('Ctrl Pts',(-208.398945412955,-66.2855529206304,
9.8491256538062));
#15995=CARTESIAN_POINT('Ctrl Pts',(-205.760209969182,-68.5535274073437,
10.0080339726105));
#15996=CARTESIAN_POINT('Ctrl Pts',(-202.66434118819,-67.6348334757972,10.155517605616));
#15997=CARTESIAN_POINT('Ctrl Pts',(-201.933276055309,-65.7989301333022,
10.25003179902));
#15998=CARTESIAN_POINT('Ctrl Pts',(-201.925849867817,-64.9972120766658,
10.2915765528225));
#15999=CARTESIAN_POINT('Ctrl Pts',(-201.921694744017,-64.9990313139748,
9.20842344717746));
#16000=CARTESIAN_POINT('Ctrl Pts',(-201.921476386658,-64.9460911648205,
9.21117646166824));
#16001=CARTESIAN_POINT('Ctrl Pts',(-201.946721039892,-63.8747674146739,
9.26689891576045));
#16002=CARTESIAN_POINT('Ctrl Pts',(-203.192942594908,-61.8472203542135,
9.3755908094541));
#16003=CARTESIAN_POINT('Ctrl Pts',(-206.671617371331,-61.7733653252889,
9.5344991282584));
#16004=CARTESIAN_POINT('Ctrl Pts',(-208.61777202504,-64.6576529027109,9.69340744706271));
#16005=CARTESIAN_POINT('Ctrl Pts',(-207.247193721282,-67.8558004725847,
9.85231576586701));
#16006=CARTESIAN_POINT('Ctrl Pts',(-203.816413330272,-68.4357820878843,
10.0112240846713));
#16007=CARTESIAN_POINT('Ctrl Pts',(-202.064218192827,-66.5160946473908,
10.1299266451081));
#16008=CARTESIAN_POINT('Ctrl Pts',(-201.924380150693,-65.2492948176156,
10.1956597659435));
#16009=CARTESIAN_POINT('Ctrl Pts',(-201.926636231845,-65.0028238856699,
10.2084234471775));
#16010=CARTESIAN_POINT('Origin',(-205.,-65.,-2.20842344717744));
#16011=CARTESIAN_POINT('',(-201.929534568487,-64.9977303426259,8.20842344717746));
#16012=CARTESIAN_POINT('',(-201.925313510444,-65.0027227882489,8.29157655282255));
#16013=CARTESIAN_POINT('',(-201.9265,-64.9999999999997,-2.20842344717744));
#16014=CARTESIAN_POINT('Ctrl Pts',(-201.925313510444,-65.0027227882489,
8.29157655282255));
#16015=CARTESIAN_POINT('Ctrl Pts',(-201.932861178308,-64.1837468504499,
8.33403463007084));
#16016=CARTESIAN_POINT('Ctrl Pts',(-202.690778756775,-62.3307071827764,
8.42946214692057));
#16017=CARTESIAN_POINT('Ctrl Pts',(-205.821270902666,-61.4600861117225,
8.57785910337174));
#16018=CARTESIAN_POINT('Ctrl Pts',(-208.420572386066,-63.7731500565804,
8.73676742217605));
#16019=CARTESIAN_POINT('Ctrl Pts',(-207.883931336951,-67.2109763173173,
8.89567574098036));
#16020=CARTESIAN_POINT('Ctrl Pts',(-204.703334271224,-68.6218042019629,
9.05458405978466));
#16021=CARTESIAN_POINT('Ctrl Pts',(-202.287845189519,-67.0359571342454,
9.18655099706539));
#16022=CARTESIAN_POINT('Ctrl Pts',(-201.931227407294,-65.504742989671,9.26554849474469));
#16023=CARTESIAN_POINT('Ctrl Pts',(-201.931440561712,-65.000145803285,9.29157655282255));
#16024=CARTESIAN_POINT('Ctrl Pts',(-201.929534568487,-64.9977303426259,
8.20842344717746));
#16025=CARTESIAN_POINT('Ctrl Pts',(-201.92711734297,-64.6440919294598,8.22669315739296));
#16026=CARTESIAN_POINT('Ctrl Pts',(-202.147019439276,-63.2680620239934,
8.29793230720989));
#16027=CARTESIAN_POINT('Ctrl Pts',(-204.178729105786,-61.4600861481526,
8.42214089662826));
#16028=CARTESIAN_POINT('Ctrl Pts',(-207.530962539076,-62.3923756815873,
8.58104921543256));
#16029=CARTESIAN_POINT('Ctrl Pts',(-208.562837804587,-65.7153060452649,
8.73995753423686));
#16030=CARTESIAN_POINT('Ctrl Pts',(-206.328343191953,-68.3824518214713,
8.89886585304117));
#16031=CARTESIAN_POINT('Ctrl Pts',(-202.935848001202,-67.9561197966926,
9.0550211573547));
#16032=CARTESIAN_POINT('Ctrl Pts',(-201.925677696523,-65.9646873409452,
9.1582070220668));
#16033=CARTESIAN_POINT('Ctrl Pts',(-201.921694744017,-64.9990313139748,
9.20842344717746));
#16034=CARTESIAN_POINT('Origin',(-205.,-65.,-2.20842344717744));
#16035=CARTESIAN_POINT('',(-201.929918496038,-65.0020818238314,7.20842344717746));
#16036=CARTESIAN_POINT('',(-201.922453576025,-64.9983309056558,7.29157655282255));
#16037=CARTESIAN_POINT('',(-201.9265,-64.9999999999997,-2.20842344717744));
#16038=CARTESIAN_POINT('Ctrl Pts',(-201.922453576025,-64.9983309056558,
7.29157655282255));
#16039=CARTESIAN_POINT('Ctrl Pts',(-201.921823116646,-64.9020160304314,
7.29658188619413));
#16040=CARTESIAN_POINT('Ctrl Pts',(-201.969645702973,-63.7870736983909,
7.35455665916714));
#16041=CARTESIAN_POINT('Ctrl Pts',(-203.328382611466,-61.7733652920829,
7.4655008717416));
#16042=CARTESIAN_POINT('Ctrl Pts',(-206.807057423689,-61.8472203217673,
7.6244091905459));
#16043=CARTESIAN_POINT('Ctrl Pts',(-208.629042186982,-64.811508522489,7.78331750935021));
#16044=CARTESIAN_POINT('Ctrl Pts',(-207.123961634304,-67.9486036030623,
7.94222582815452));
#16045=CARTESIAN_POINT('Ctrl Pts',(-203.671656794376,-68.3824518562811,
8.10113414695882));
#16046=CARTESIAN_POINT('Ctrl Pts',(-202.034187830935,-66.4279300575628,
8.21758438851483));
#16047=CARTESIAN_POINT('Ctrl Pts',(-201.923444931436,-65.2054769730502,
8.28106519046941));
#16048=CARTESIAN_POINT('Ctrl Pts',(-201.925313510444,-65.0027227882489,
8.29157655282255));
#16049=CARTESIAN_POINT('Ctrl Pts',(-201.929918496038,-65.0020818238314,
7.20842344717746));
#16050=CARTESIAN_POINT('Ctrl Pts',(-201.933986215544,-64.3478883205901,
7.24220985311768));
#16051=CARTESIAN_POINT('Ctrl Pts',(-202.459399639161,-62.6621016376928,
7.32896569865933));
#16052=CARTESIAN_POINT('Ctrl Pts',(-205.234272799839,-61.3736254722602,
7.46869098380241));
#16053=CARTESIAN_POINT('Ctrl Pts',(-208.175332576579,-63.2328726734323,
7.62759930260673));
#16054=CARTESIAN_POINT('Ctrl Pts',(-208.205282937147,-66.7122024567848,
7.78650762141103));
#16055=CARTESIAN_POINT('Ctrl Pts',(-205.296665725724,-68.62180416469,7.94541594021533));
#16056=CARTESIAN_POINT('Ctrl Pts',(-202.481742349981,-67.3731793594825,
8.08605454880414));
#16057=CARTESIAN_POINT('Ctrl Pts',(-201.93412561401,-65.6693971119722,8.17372371779152));
#16058=CARTESIAN_POINT('Ctrl Pts',(-201.929534568487,-64.9977303426259,
8.20842344717746));
#16059=CARTESIAN_POINT('Origin',(-205.,-65.,-2.20842344717744));
#16060=CARTESIAN_POINT('',(-201.92196047901,-65.0012666663909,6.20842344717746));
#16061=CARTESIAN_POINT('',(-201.93041282103,-64.9982329274285,6.29157655282255));
#16062=CARTESIAN_POINT('',(-201.9265,-64.9999999999997,-2.20842344717744));
#16063=CARTESIAN_POINT('Ctrl Pts',(-201.93041282103,-64.9982329274285,6.29157655282255));
#16064=CARTESIAN_POINT('Ctrl Pts',(-201.928336237733,-64.6007120797469,
6.31209858191885));
#16065=CARTESIAN_POINT('Ctrl Pts',(-202.184897914724,-63.1797266043789,
6.38559005061658));
#16066=CARTESIAN_POINT('Ctrl Pts',(-204.329711780416,-61.428419126679,6.51205095891576));
#16067=CARTESIAN_POINT('Ctrl Pts',(-207.639355934117,-62.5021456237346,
6.67095927772006));
#16068=CARTESIAN_POINT('Ctrl Pts',(-208.529268066955,-65.8658770949486,
6.82986759652438));
#16069=CARTESIAN_POINT('Ctrl Pts',(-206.183586681908,-68.4357821232429,
6.98877591532867));
#16070=CARTESIAN_POINT('Ctrl Pts',(-202.860869822607,-67.8740689059555,
7.14267890076141));
#16071=CARTESIAN_POINT('Ctrl Pts',(-201.928495015897,-65.9212778032609,
7.24361244659269));
#16072=CARTESIAN_POINT('Ctrl Pts',(-201.922453576025,-64.9983309056558,
7.29157655282255));
#16073=CARTESIAN_POINT('Ctrl Pts',(-201.92196047901,-65.0012666663909,6.20842344717746));
#16074=CARTESIAN_POINT('Ctrl Pts',(-201.926898060984,-64.052956064959,6.25772654884239));
#16075=CARTESIAN_POINT('Ctrl Pts',(-202.905060811709,-62.0770176673835,
6.35999909010877));
#16076=CARTESIAN_POINT('Ctrl Pts',(-206.26991780915,-61.5951821314221,6.51524107097657));
#16077=CARTESIAN_POINT('Ctrl Pts',(-208.549995921993,-64.2234660895895,
6.67414938978088));
#16078=CARTESIAN_POINT('Ctrl Pts',(-207.575477451123,-67.5636676576622,
6.83305770858519));
#16079=CARTESIAN_POINT('Ctrl Pts',(-204.239790038642,-68.5535273707736,
6.9919660273895));
#16080=CARTESIAN_POINT('Ctrl Pts',(-202.162091241287,-66.7677599212191,
7.11708794025358));
#16081=CARTESIAN_POINT('Ctrl Pts',(-201.927608951769,-65.3735157080934,
7.18924041351624));
#16082=CARTESIAN_POINT('Ctrl Pts',(-201.929918496038,-65.0020818238314,
7.20842344717746));
#16083=CARTESIAN_POINT('Origin',(-205.,-65.,-2.20842344717744));
#16084=CARTESIAN_POINT('',(-201.926100533607,-64.9971929803835,5.20842344717745));
#16085=CARTESIAN_POINT('',(-201.928910873452,-65.0025004618091,5.29157655282255));
#16086=CARTESIAN_POINT('',(-201.9265,-64.9999999999997,-2.20842344717744));
#16087=CARTESIAN_POINT('Ctrl Pts',(-201.928910873452,-65.0025004618091,
5.29157655282255));
#16088=CARTESIAN_POINT('Ctrl Pts',(-201.934235624731,-64.3052721134968,
5.32761527764357));
#16089=CARTESIAN_POINT('Ctrl Pts',(-202.515343946683,-62.5752315257807,
5.41662344206602));
#16090=CARTESIAN_POINT('Ctrl Pts',(-205.387973952159,-61.3868362278423,
5.55860104608991));
#16091=CARTESIAN_POINT('Ctrl Pts',(-208.247472586089,-63.3692339117493,
5.71750936489423));
#16092=CARTESIAN_POINT('Ctrl Pts',(-208.129724649422,-66.8466997186291,
5.87641768369853));
#16093=CARTESIAN_POINT('Ctrl Pts',(-205.142680134451,-68.6311318636507,
6.03532600250283));
#16094=CARTESIAN_POINT('Ctrl Pts',(-202.427479427965,-67.286051871031,6.17371229221084));
#16095=CARTESIAN_POINT('Ctrl Pts',(-201.933696109946,-65.6267537266412,
6.25912914231741));
#16096=CARTESIAN_POINT('Ctrl Pts',(-201.93041282103,-64.9982329274285,6.29157655282255));
#16097=CARTESIAN_POINT('Ctrl Pts',(-201.926100533607,-64.9971929803835,
5.20842344717745));
#16098=CARTESIAN_POINT('Ctrl Pts',(-201.923984660047,-64.7684605820622,
5.22027380496568));
#16099=CARTESIAN_POINT('Ctrl Pts',(-202.051779336195,-63.5196687889702,
5.28509360235533));
#16100=CARTESIAN_POINT('Ctrl Pts',(-203.757442108639,-61.5851023665706,
5.40288283934643));
#16101=CARTESIAN_POINT('Ctrl Pts',(-207.197698422129,-62.1059375256302,
5.56179115815073));
#16102=CARTESIAN_POINT('Ctrl Pts',(-208.623129385432,-65.2800168148538,
5.72069947695504));
#16103=CARTESIAN_POINT('Ctrl Pts',(-206.726915823139,-68.1973798179096,
5.87960779575935));
#16104=CARTESIAN_POINT('Ctrl Pts',(-203.247485135573,-68.183420740359,6.03851611456365));
#16105=CARTESIAN_POINT('Ctrl Pts',(-201.955780678157,-66.1607732940332,
6.14812133170302));
#16106=CARTESIAN_POINT('Ctrl Pts',(-201.921593304462,-65.0717861066736,
6.20475710924096));
#16107=CARTESIAN_POINT('Ctrl Pts',(-201.92196047901,-65.0012666663909,6.20842344717746));
#16108=CARTESIAN_POINT('Origin',(-205.,-65.,-2.20842344717744));
#16109=CARTESIAN_POINT('',(-201.931423553656,-65.0002813807169,4.20842344717746));
#16110=CARTESIAN_POINT('',(-201.921426613004,-65.0005065231376,4.29157655282254));
#16111=CARTESIAN_POINT('',(-201.9265,-64.9999999999997,-2.20842344717744));
#16112=CARTESIAN_POINT('Ctrl Pts',(-201.921426613004,-65.0005065231376,
4.29157655282254));
#16113=CARTESIAN_POINT('Ctrl Pts',(-201.923689481612,-64.0093326254348,
4.34313197336828));
#16114=CARTESIAN_POINT('Ctrl Pts',(-202.981935532719,-61.9956495212633,
4.44765683351546));
#16115=CARTESIAN_POINT('Ctrl Pts',(-206.413282356468,-61.652148567679,4.60515113326408));
#16116=CARTESIAN_POINT('Ctrl Pts',(-208.579755111172,-64.3748363606043,
4.76405945206838));
#16117=CARTESIAN_POINT('Ctrl Pts',(-207.464348390136,-67.6706671908,4.92296777087269));
#16118=CARTESIAN_POINT('Ctrl Pts',(-204.089654608536,-68.5180601899667,
5.08187608967699));
#16119=CARTESIAN_POINT('Ctrl Pts',(-202.125622944275,-66.6794232091735,
5.20474568366028));
#16120=CARTESIAN_POINT('Ctrl Pts',(-201.926409346397,-65.3300529587612,
5.27464583804213));
#16121=CARTESIAN_POINT('Ctrl Pts',(-201.928910873452,-65.0025004618091,
5.29157655282255));
#16122=CARTESIAN_POINT('Ctrl Pts',(-201.931423553656,-65.0002813807169,
4.20842344717746));
#16123=CARTESIAN_POINT('Ctrl Pts',(-201.931856208338,-64.4697328931174,
4.2357905006904));
#16124=CARTESIAN_POINT('Ctrl Pts',(-202.315183154355,-62.9117123239822,
4.31612699380478));
#16125=CARTESIAN_POINT('Ctrl Pts',(-204.794831471885,-61.3718624839552,
4.44943292652058));
#16126=CARTESIAN_POINT('Ctrl Pts',(-207.93881072326,-62.8625090659739,4.6083412453249));
#16127=CARTESIAN_POINT('Ctrl Pts',(-208.388521150012,-66.3127834459959,
4.7672495641292));
#16128=CARTESIAN_POINT('Ctrl Pts',(-205.731673259242,-68.5595126354467,
4.92615788293351));
#16129=CARTESIAN_POINT('Ctrl Pts',(-202.652189269735,-67.6187313168277,
5.07321584394959));
#16130=CARTESIAN_POINT('Ctrl Pts',(-201.93344231852,-65.7908623672484,5.16730436536424));
#16131=CARTESIAN_POINT('Ctrl Pts',(-201.926100533607,-64.9971929803835,
5.20842344717745));
#16132=CARTESIAN_POINT('Origin',(-205.,-65.,-2.20842344717744));
#16133=CARTESIAN_POINT('',(-201.925065525565,-65.0026812057629,3.20842344717745));
#16134=CARTESIAN_POINT('',(-201.927406805321,-64.9972100888671,3.29157655282254));
#16135=CARTESIAN_POINT('',(-201.9265,-64.9999999999997,-2.20842344717744));
#16136=CARTESIAN_POINT('Ctrl Pts',(-201.927406805321,-64.9972100888671,
3.29157655282254));
#16137=CARTESIAN_POINT('Ctrl Pts',(-201.924995747753,-64.724708687099,3.30567922949157));
#16138=CARTESIAN_POINT('Ctrl Pts',(-202.083109157865,-63.4314473629371,
3.37275134576203));
#16139=CARTESIAN_POINT('Ctrl Pts',(-203.90349839961,-61.5354422402711,3.49279290163393));
#16140=CARTESIAN_POINT('Ctrl Pts',(-207.318549253241,-62.2018210220118,
3.65170122043824));
#16141=CARTESIAN_POINT('Ctrl Pts',(-208.607980065528,-65.4335390165435,
3.81060953924254));
#16142=CARTESIAN_POINT('Ctrl Pts',(-206.589655079347,-68.2677932860708,
3.96951785804685));
#16143=CARTESIAN_POINT('Ctrl Pts',(-203.113952083686,-68.1061711944818,
4.12842617685116));
#16144=CARTESIAN_POINT('Ctrl Pts',(-201.934013400269,-66.0731764684801,
4.23577907510972));
#16145=CARTESIAN_POINT('Ctrl Pts',(-201.921364548932,-65.0276916137454,
4.29016253376685));
#16146=CARTESIAN_POINT('Ctrl Pts',(-201.921426613004,-65.0005065231376,
4.29157655282254));
#16147=CARTESIAN_POINT('Ctrl Pts',(-201.925065525565,-65.0026812057629,
3.20842344717745));
#16148=CARTESIAN_POINT('Ctrl Pts',(-201.932639942483,-64.1756663036064,
3.25130719641512));
#16149=CARTESIAN_POINT('Ctrl Pts',(-202.703271098363,-62.3146899905717,
3.34716038525422));
#16150=CARTESIAN_POINT('Ctrl Pts',(-205.849647457805,-61.4667896805192,
3.49598301369474));
#16151=CARTESIAN_POINT('Ctrl Pts',(-208.430306047719,-63.8006350093353,
3.65489133249905));
#16152=CARTESIAN_POINT('Ctrl Pts',(-207.86609839156,-67.2340447552034,3.81379965130336));
#16153=CARTESIAN_POINT('Ctrl Pts',(-204.674283764462,-68.6193072396057,
3.97270797010767));
#16154=CARTESIAN_POINT('Ctrl Pts',(-202.27934682778,-67.0193078694193,4.10424923539903));
#16155=CARTESIAN_POINT('Ctrl Pts',(-201.931018797178,-65.4966193299875,
4.18282106108896));
#16156=CARTESIAN_POINT('Ctrl Pts',(-201.931423553656,-65.0002813807169,
4.20842344717746));
#16157=CARTESIAN_POINT('Origin',(-205.,-65.,-2.20842344717744));
#16158=CARTESIAN_POINT('',(-201.922632855754,-64.9982129720012,2.20842344717745));
#16159=CARTESIAN_POINT('',(-201.931155097516,-65.0009810679335,2.29157655282254));
#16160=CARTESIAN_POINT('',(-201.9265,-64.9999999999997,-2.20842344717744));
#16161=CARTESIAN_POINT('Ctrl Pts',(-201.931155097516,-65.0009810679335,
2.29157655282254));
#16162=CARTESIAN_POINT('Ctrl Pts',(-201.932795742513,-64.4268935344444,
2.32119592521629));
#16163=CARTESIAN_POINT('Ctrl Pts',(-202.363272159361,-62.8238592626871,
2.40378473721147));
#16164=CARTESIAN_POINT('Ctrl Pts',(-204.949003423762,-61.3664238768246,
2.53934298880808));
#16165=CARTESIAN_POINT('Ctrl Pts',(-208.026882997387,-62.9891654522027,
2.69825130761239));
#16166=CARTESIAN_POINT('Ctrl Pts',(-208.329750076191,-66.455417699762,2.8571596264167));
#16167=CARTESIAN_POINT('Ctrl Pts',(-205.579939497992,-68.5873592508376,
3.01606794522101));
#16168=CARTESIAN_POINT('Ctrl Pts',(-202.589670325603,-67.5331224660227,
3.16087358735629));
#16169=CARTESIAN_POINT('Ctrl Pts',(-201.9340516434,-65.7482198177174,3.25270978989013));
#16170=CARTESIAN_POINT('Ctrl Pts',(-201.927406805321,-64.9972100888671,
3.29157655282254));
#16171=CARTESIAN_POINT('Ctrl Pts',(-201.922632855754,-64.9982129720012,
2.20842344717745));
#16172=CARTESIAN_POINT('Ctrl Pts',(-201.921910441958,-64.8936910841268,
2.2138544525384));
#16173=CARTESIAN_POINT('Ctrl Pts',(-201.974200188913,-63.7704822827847,
2.27225489750078));
#16174=CARTESIAN_POINT('Ctrl Pts',(-203.354325918685,-61.7600568500266,
2.3836247820646));
#16175=CARTESIAN_POINT('Ctrl Pts',(-206.832295952684,-61.8618209657714,
2.54253310086891));
#16176=CARTESIAN_POINT('Ctrl Pts',(-208.630437747347,-64.8406327545204,
2.70144141967322));
#16177=CARTESIAN_POINT('Ctrl Pts',(-207.100234689454,-67.965550551091,2.86034973847752));
#16178=CARTESIAN_POINT('Ctrl Pts',(-203.644559991919,-68.3716847971282,
3.01925805728183));
#16179=CARTESIAN_POINT('Ctrl Pts',(-202.028754213716,-66.4112798143637,
3.13528262684847));
#16180=CARTESIAN_POINT('Ctrl Pts',(-201.923284122934,-65.1971841673195,
3.19833775681368));
#16181=CARTESIAN_POINT('Ctrl Pts',(-201.925065525565,-65.0026812057629,
3.20842344717745));
#16182=CARTESIAN_POINT('Origin',(-205.,-65.,-2.20842344717744));
#16183=CARTESIAN_POINT('',(-201.930556952874,-64.9983469618497,1.20842344717745));
#16184=CARTESIAN_POINT('',(-201.92380386931,-65.0023470817023,1.29157655282254));
#16185=CARTESIAN_POINT('',(-201.9265,-64.9999999999997,-2.20842344717744));
#16186=CARTESIAN_POINT('Ctrl Pts',(-201.92380386931,-65.0023470817023,1.29157655282254));
#16187=CARTESIAN_POINT('Ctrl Pts',(-201.931157820393,-64.1328208103926,
1.33671262094101));
#16188=CARTESIAN_POINT('Ctrl Pts',(-202.771191487033,-62.2304278274959,
1.43481812866091));
#16189=CARTESIAN_POINT('Ctrl Pts',(-205.998840266797,-61.5060359469962,
1.58589307598225));
#16190=CARTESIAN_POINT('Ctrl Pts',(-208.478118943853,-63.9473056488985,
1.74480139478655));
#16191=CARTESIAN_POINT('Ctrl Pts',(-207.768697529891,-67.3536763121769,
1.90370971359086));
#16192=CARTESIAN_POINT('Ctrl Pts',(-204.52096493132,-68.6022216022895,2.06261803239517));
#16193=CARTESIAN_POINT('Ctrl Pts',(-202.235901628419,-66.931128943739,2.19190697880573));
#16194=CARTESIAN_POINT('Ctrl Pts',(-201.929861715252,-65.453555900103,2.26822648561485));
#16195=CARTESIAN_POINT('Ctrl Pts',(-201.931155097516,-65.0009810679335,
2.29157655282254));
#16196=CARTESIAN_POINT('Ctrl Pts',(-201.930556952874,-64.9983469618497,
1.20842344717745));
#16197=CARTESIAN_POINT('Ctrl Pts',(-201.928569491267,-64.5925310316569,
1.22937114826312));
#16198=CARTESIAN_POINT('Ctrl Pts',(-202.192314055039,-63.1630216590503,
1.30328828895022));
#16199=CARTESIAN_POINT('Ctrl Pts',(-204.358399560164,-61.4231650176065,
1.43017486923876));
#16200=CARTESIAN_POINT('Ctrl Pts',(-207.659308409489,-62.5233989116837,
1.58908318804307));
#16201=CARTESIAN_POINT('Ctrl Pts',(-208.522209085787,-65.8941689287448,
1.74799150684737));
#16202=CARTESIAN_POINT('Ctrl Pts',(-206.155980040914,-68.445167130006,1.90689982565168));
#16203=CARTESIAN_POINT('Ctrl Pts',(-202.847056020182,-67.8584404971801,
2.06037713909504));
#16204=CARTESIAN_POINT('Ctrl Pts',(-201.928956256023,-65.9131093057697,
2.16088501293696));
#16205=CARTESIAN_POINT('Ctrl Pts',(-201.922632855754,-64.9982129720012,
2.20842344717745));
#16206=CARTESIAN_POINT('Origin',(-205.,-65.,-2.20842344717744));
#16207=CARTESIAN_POINT('',(-201.92961158086,-65.0031570762977,0.208423447177454));
#16208=CARTESIAN_POINT('',(-201.923731533573,-64.9977249101301,0.291576552822544));
#16209=CARTESIAN_POINT('',(-201.9265,-64.9999999999997,-2.20842344717744));
#16210=CARTESIAN_POINT('',(-204.206200717467,-67.9692229537457,0.));
#16211=CARTESIAN_POINT('Ctrl Pts',(-204.206200717467,-67.9692229537457,
-8.32667268468867E-16));
#16212=CARTESIAN_POINT('Ctrl Pts',(-203.217993421758,-67.705033213013,0.0529694396014348));
#16213=CARTESIAN_POINT('Ctrl Pts',(-202.119878302883,-66.6624875897336,
0.12244392199392));
#16214=CARTESIAN_POINT('Ctrl Pts',(-201.92719206015,-65.3223930798511,0.191918404386405));
#16215=CARTESIAN_POINT('Ctrl Pts',(-201.92961158086,-65.0031570762977,0.208423447177454));
#16216=CARTESIAN_POINT('',(-205.795567289133,-67.9745804941197,-1.17835206387761E-15));
#16217=CARTESIAN_POINT('Origin',(-205.,-65.,0.));
#16218=CARTESIAN_POINT('Ctrl Pts',(-205.795568749511,-67.9745849194644,
-1.60597446799415E-16));
#16219=CARTESIAN_POINT('Ctrl Pts',(-204.83119279379,-68.2310729434654,0.0519060689144953));
#16220=CARTESIAN_POINT('Ctrl Pts',(-202.766529390716,-67.7537239905742,
0.149098253188677));
#16221=CARTESIAN_POINT('Ctrl Pts',(-201.931014089346,-65.8699107350031,
0.246290437462858));
#16222=CARTESIAN_POINT('Ctrl Pts',(-201.923731533573,-64.9977249101301,
0.291576552822544));
#16223=CARTESIAN_POINT('Origin',(-205.,-65.,17.));
#16224=CARTESIAN_POINT('Ctrl Pts',(-203.086534003335,-63.3640127966251,
17.));
#16225=CARTESIAN_POINT('Ctrl Pts',(-203.02440597855,-63.4223978842397,17.));
#16226=CARTESIAN_POINT('Ctrl Pts',(-202.965656533056,-63.484037682377,17.));
#16227=CARTESIAN_POINT('Ctrl Pts',(-202.910296296302,-63.5485554899634,
17.));
#16228=CARTESIAN_POINT('Ctrl Pts',(-202.853579007623,-63.6146548300752,
17.));
#16229=CARTESIAN_POINT('Ctrl Pts',(-202.800418658262,-63.6837754979915,
17.));
#16230=CARTESIAN_POINT('Ctrl Pts',(-202.750855616275,-63.7555586853473,
17.));
#16231=CARTESIAN_POINT('Ctrl Pts',(-202.737942375479,-63.7742612013012,
17.));
#16232=CARTESIAN_POINT('Ctrl Pts',(-202.725273497568,-63.7931446704172,
17.));
#16233=CARTESIAN_POINT('Ctrl Pts',(-202.712850070252,-63.8122031777925,
17.));
#16234=CARTESIAN_POINT('Ctrl Pts',(-202.702648305927,-63.8278534807001,
17.));
#16235=CARTESIAN_POINT('Ctrl Pts',(-202.692611588147,-63.8436227659743,
17.));
#16236=CARTESIAN_POINT('Ctrl Pts',(-202.682749443169,-63.859493035454,17.));
#16237=CARTESIAN_POINT('Ctrl Pts',(-202.63531796322,-63.9358202817403,17.));
#16238=CARTESIAN_POINT('Ctrl Pts',(-202.59187124907,-64.0145559081911,17.));
#16239=CARTESIAN_POINT('Ctrl Pts',(-202.552442526139,-64.0953069128711,
17.));
#16240=CARTESIAN_POINT('Ctrl Pts',(-202.520315679276,-64.1611034938538,
17.));
#16241=CARTESIAN_POINT('Ctrl Pts',(-202.490856911205,-64.2282391982212,
17.));
#16242=CARTESIAN_POINT('Ctrl Pts',(-202.464101958719,-64.2965198329108,
17.));
#16243=CARTESIAN_POINT('Ctrl Pts',(-202.455216196125,-64.3191969619356,
17.));
#16244=CARTESIAN_POINT('Ctrl Pts',(-202.446628808742,-64.3420004925349,
17.));
#16245=CARTESIAN_POINT('Ctrl Pts',(-202.43834153865,-64.3649236233451,17.));
#16246=CARTESIAN_POINT('Ctrl Pts',(-202.431659599736,-64.3834063031797,
17.));
#16247=CARTESIAN_POINT('Ctrl Pts',(-202.425171976069,-64.4019694556671,
17.));
#16248=CARTESIAN_POINT('Ctrl Pts',(-202.418887257457,-64.4205860790577,
17.));
#16249=CARTESIAN_POINT('Ctrl Pts',(-202.389370048133,-64.5080220970403,
17.));
#16250=CARTESIAN_POINT('Ctrl Pts',(-202.364286527296,-64.5967387245119,
17.));
#16251=CARTESIAN_POINT('Ctrl Pts',(-202.343667851554,-64.6863376891691,
17.));
#16252=CARTESIAN_POINT('Ctrl Pts',(-202.322591412091,-64.7779258773834,
17.));
#16253=CARTESIAN_POINT('Ctrl Pts',(-202.306179715118,-64.8704368052643,
17.));
#16254=CARTESIAN_POINT('Ctrl Pts',(-202.294508870619,-64.9634790031726,
17.));
#16255=CARTESIAN_POINT('Ctrl Pts',(-202.283005247673,-65.0551880789642,
17.));
#16256=CARTESIAN_POINT('Ctrl Pts',(-202.276107302816,-65.1474142708408,
17.));
#16257=CARTESIAN_POINT('Ctrl Pts',(-202.273935013967,-65.2398018803324,
17.));
#16258=CARTESIAN_POINT('Ctrl Pts',(-202.272809982513,-65.2876495533737,
17.));
#16259=CARTESIAN_POINT('Ctrl Pts',(-202.272953276915,-65.3355407504061,
17.));
#16260=CARTESIAN_POINT('Ctrl Pts',(-202.27438704446,-65.383426836211,17.));
#16261=CARTESIAN_POINT('Ctrl Pts',(-202.275036744558,-65.4051260264126,
17.));
#16262=CARTESIAN_POINT('Ctrl Pts',(-202.275952004537,-65.4268312379048,
17.));
#16263=CARTESIAN_POINT('Ctrl Pts',(-202.277132662655,-65.4484998374491,
17.));
#16264=CARTESIAN_POINT('Ctrl Pts',(-202.282342582934,-65.5441174209293,
17.));
#16265=CARTESIAN_POINT('Ctrl Pts',(-202.292716438461,-65.6391274226978,
17.));
#16266=CARTESIAN_POINT('Ctrl Pts',(-202.308321259936,-65.7331327397659,
17.));
#16267=CARTESIAN_POINT('Ctrl Pts',(-202.312170275657,-65.7563196723322,
17.));
#16268=CARTESIAN_POINT('Ctrl Pts',(-202.316337767864,-65.7794455742674,
17.));
#16269=CARTESIAN_POINT('Ctrl Pts',(-202.320825205417,-65.8025046417956,
17.));
#16270=CARTESIAN_POINT('Ctrl Pts',(-202.338330039074,-65.8924546715381,
17.));
#16271=CARTESIAN_POINT('Ctrl Pts',(-202.360699143547,-65.981387621661,17.));
#16272=CARTESIAN_POINT('Ctrl Pts',(-202.387629324862,-66.0690734250235,
17.));
#16273=CARTESIAN_POINT('Ctrl Pts',(-202.415161796534,-66.1587203111241,
17.));
#16274=CARTESIAN_POINT('Ctrl Pts',(-202.447461860745,-66.2470643438459,
17.));
#16275=CARTESIAN_POINT('Ctrl Pts',(-202.484259699373,-66.3338552345522,
17.));
#16276=CARTESIAN_POINT('Ctrl Pts',(-202.498888789869,-66.3683592120058,
17.));
#16277=CARTESIAN_POINT('Ctrl Pts',(-202.514229318749,-66.4026176104445,
17.));
#16278=CARTESIAN_POINT('Ctrl Pts',(-202.53026650595,-66.4366141224841,17.));
#16279=CARTESIAN_POINT('Ctrl Pts',(-202.538263030882,-66.4535655961273,
17.));
#16280=CARTESIAN_POINT('Ctrl Pts',(-202.546434613239,-66.4704554166591,
17.));
#16281=CARTESIAN_POINT('Ctrl Pts',(-202.554767107621,-66.4872571600793,
17.));
#16282=CARTESIAN_POINT('Ctrl Pts',(-202.597562057197,-66.5735494189751,
17.));
#16283=CARTESIAN_POINT('Ctrl Pts',(-202.644652245067,-66.6576403398475,
17.));
#16284=CARTESIAN_POINT('Ctrl Pts',(-202.695692225863,-66.7392833372882,
17.));
#16285=CARTESIAN_POINT('Ctrl Pts',(-202.747749531408,-66.8225536363186,
17.));
#16286=CARTESIAN_POINT('Ctrl Pts',(-202.803915970958,-66.9032782223774,
17.));
#16287=CARTESIAN_POINT('Ctrl Pts',(-202.863880125944,-66.9811882726074,
17.));
#16288=CARTESIAN_POINT('Ctrl Pts',(-202.924342162766,-67.0597452092798,
17.));
#16289=CARTESIAN_POINT('Ctrl Pts',(-202.988665705321,-67.1354415100437,
17.));
#16290=CARTESIAN_POINT('Ctrl Pts',(-203.056580879016,-67.2079822210047,
17.));
#16291=CARTESIAN_POINT('Ctrl Pts',(-203.094627114409,-67.2486196929359,
17.));
#16292=CARTESIAN_POINT('Ctrl Pts',(-203.13380134389,-67.2882664402971,17.));
#16293=CARTESIAN_POINT('Ctrl Pts',(-203.17406195576,-67.326866466561,17.));
#16294=CARTESIAN_POINT('Ctrl Pts',(-203.185603488747,-67.3379319585079,
17.));
#16295=CARTESIAN_POINT('Ctrl Pts',(-203.197234324745,-67.3489114087184,
17.));
#16296=CARTESIAN_POINT('Ctrl Pts',(-203.208953539895,-67.3598034420083,
17.));
#16297=CARTESIAN_POINT('Ctrl Pts',(-203.219358840357,-67.3694743011535,
17.));
#16298=CARTESIAN_POINT('Ctrl Pts',(-203.229830604016,-67.3790732118472,
17.));
#16299=CARTESIAN_POINT('Ctrl Pts',(-203.240361997973,-67.3885939838815,
17.));
#16300=CARTESIAN_POINT('Ctrl Pts',(-203.316072549381,-67.457039139711,17.));
#16301=CARTESIAN_POINT('Ctrl Pts',(-203.394952319029,-67.5215327177357,
17.));
#16302=CARTESIAN_POINT('Ctrl Pts',(-203.476670785051,-67.5817955879554,
17.));
#16303=CARTESIAN_POINT('Ctrl Pts',(-203.558482237366,-67.6421270304475,
17.));
#16304=CARTESIAN_POINT('Ctrl Pts',(-203.643139431469,-67.6982189644735,
17.));
#16305=CARTESIAN_POINT('Ctrl Pts',(-203.730355930017,-67.7497653639998,
17.));
#16306=CARTESIAN_POINT('Ctrl Pts',(-203.815753640172,-67.8002368293722,
17.));
#16307=CARTESIAN_POINT('Ctrl Pts',(-203.903605699369,-67.8463510305609,
17.));
#16308=CARTESIAN_POINT('Ctrl Pts',(-203.993677035266,-67.8877849551271,
17.));
#16309=CARTESIAN_POINT('Ctrl Pts',(-204.044060944389,-67.9109621742627,
17.));
#16310=CARTESIAN_POINT('Ctrl Pts',(-204.095139826534,-67.9326742194188,
17.));
#16311=CARTESIAN_POINT('Ctrl Pts',(-204.146876136319,-67.9528583341107,
17.));
#16312=CARTESIAN_POINT('Ctrl Pts',(-204.165972573965,-67.9603085115445,
17.));
#16313=CARTESIAN_POINT('Ctrl Pts',(-204.185158603728,-67.9675504698475,
17.));
#16314=CARTESIAN_POINT('Ctrl Pts',(-204.204431258832,-67.9745848956374,
17.));
#16315=CARTESIAN_POINT('Ctrl Pts',(-205.793799282533,-67.9692229537457,
17.));
#16316=CARTESIAN_POINT('Ctrl Pts',(-205.888627148018,-67.9345344969579,
17.));
#16317=CARTESIAN_POINT('Ctrl Pts',(-205.981409263194,-67.8948513145698,
17.));
#16318=CARTESIAN_POINT('Ctrl Pts',(-206.071905763361,-67.8504949414992,
17.));
#16319=CARTESIAN_POINT('Ctrl Pts',(-206.16368767609,-67.8055085303715,17.));
#16320=CARTESIAN_POINT('Ctrl Pts',(-206.253119250409,-67.7557145264303,
17.));
#16321=CARTESIAN_POINT('Ctrl Pts',(-206.339916218874,-67.701407654434,17.));
#16322=CARTESIAN_POINT('Ctrl Pts',(-206.364296575079,-67.6861534248557,
17.));
#16323=CARTESIAN_POINT('Ctrl Pts',(-206.388468826147,-67.6705429272934,
17.));
#16324=CARTESIAN_POINT('Ctrl Pts',(-206.412426086333,-67.6545822455055,
17.));
#16325=CARTESIAN_POINT('Ctrl Pts',(-206.431863526899,-67.6416327345333,
17.));
#16326=CARTESIAN_POINT('Ctrl Pts',(-206.451161651935,-67.6284510097797,
17.));
#16327=CARTESIAN_POINT('Ctrl Pts',(-206.470297235862,-67.6150542711723,
17.));
#16328=CARTESIAN_POINT('Ctrl Pts',(-206.553008824826,-67.5571482495228,
17.));
#16329=CARTESIAN_POINT('Ctrl Pts',(-206.632764547703,-67.495177621976,17.));
#16330=CARTESIAN_POINT('Ctrl Pts',(-206.709298974822,-67.4294411381943,
17.));
#16331=CARTESIAN_POINT('Ctrl Pts',(-206.768827144667,-67.378311565284,17.));
#16332=CARTESIAN_POINT('Ctrl Pts',(-206.826405917082,-67.3249028587324,
17.));
#16333=CARTESIAN_POINT('Ctrl Pts',(-206.881892272758,-67.2693434657245,
17.));
#16334=CARTESIAN_POINT('Ctrl Pts',(-206.912069662648,-67.2391263529871,
17.));
#16335=CARTESIAN_POINT('Ctrl Pts',(-206.941627832692,-67.2082729188649,
17.));
#16336=CARTESIAN_POINT('Ctrl Pts',(-206.970541519969,-67.1768029072482,
17.));
#16337=CARTESIAN_POINT('Ctrl Pts',(-206.982346348857,-67.1639543867987,
17.));
#16338=CARTESIAN_POINT('Ctrl Pts',(-206.994038644047,-67.1510085536672,
17.));
#16339=CARTESIAN_POINT('Ctrl Pts',(-207.005612030979,-67.1379726476749,
17.));
#16340=CARTESIAN_POINT('Ctrl Pts',(-207.071011723905,-67.0643084511959,
17.));
#16341=CARTESIAN_POINT('Ctrl Pts',(-207.132669244518,-66.9877146035452,
17.));
#16342=CARTESIAN_POINT('Ctrl Pts',(-207.190339462795,-66.9084693768327,
17.));
#16343=CARTESIAN_POINT('Ctrl Pts',(-207.247552243663,-66.8298527194637,
17.));
#16344=CARTESIAN_POINT('Ctrl Pts',(-207.300841167328,-66.7486257942039,
17.));
#16345=CARTESIAN_POINT('Ctrl Pts',(-207.349920589594,-66.6650384656478,
17.));
#16346=CARTESIAN_POINT('Ctrl Pts',(-207.397481339409,-66.5840375932332,
17.));
#16347=CARTESIAN_POINT('Ctrl Pts',(-207.44108925285,-66.500819434757,17.));
#16348=CARTESIAN_POINT('Ctrl Pts',(-207.480436480452,-66.4156016691333,
17.));
#16349=CARTESIAN_POINT('Ctrl Pts',(-207.501052397794,-66.3709519563276,
17.));
#16350=CARTESIAN_POINT('Ctrl Pts',(-207.520497841185,-66.3257532073699,
17.));
#16351=CARTESIAN_POINT('Ctrl Pts',(-207.538722766342,-66.280036559567,17.));
#16352=CARTESIAN_POINT('Ctrl Pts',(-207.545019324992,-66.2642418415239,
17.));
#16353=CARTESIAN_POINT('Ctrl Pts',(-207.551170160701,-66.2483853062549,
17.));
#16354=CARTESIAN_POINT('Ctrl Pts',(-207.557173092316,-66.2324682453042,
17.));
#16355=CARTESIAN_POINT('Ctrl Pts',(-207.562735046531,-66.2177204570677,
17.));
#16356=CARTESIAN_POINT('Ctrl Pts',(-207.568167259183,-66.2029279237178,
17.));
#16357=CARTESIAN_POINT('Ctrl Pts',(-207.573465901499,-66.1880990080578,
17.));
#16358=CARTESIAN_POINT('Ctrl Pts',(-207.604700042699,-66.1006863430889,
17.));
#16359=CARTESIAN_POINT('Ctrl Pts',(-207.631326666905,-66.0119317997892,
17.));
#16360=CARTESIAN_POINT('Ctrl Pts',(-207.653093540636,-65.9220590100927,
17.));
#16361=CARTESIAN_POINT('Ctrl Pts',(-207.65825467588,-65.9007493067314,17.));
#16362=CARTESIAN_POINT('Ctrl Pts',(-207.663142365404,-65.8793766928838,
17.));
#16363=CARTESIAN_POINT('Ctrl Pts',(-207.667752815749,-65.8579440884434,
17.));
#16364=CARTESIAN_POINT('Ctrl Pts',(-207.687563008922,-65.7658524265826,
17.));
#16365=CARTESIAN_POINT('Ctrl Pts',(-207.702258795435,-65.6726527986311,
17.));
#16366=CARTESIAN_POINT('Ctrl Pts',(-207.711951637232,-65.5787373627011,
17.));
#16367=CARTESIAN_POINT('Ctrl Pts',(-207.722120050741,-65.480214039264,17.));
#16368=CARTESIAN_POINT('Ctrl Pts',(-207.726782566171,-65.3809016624173,
17.));
#16369=CARTESIAN_POINT('Ctrl Pts',(-207.726009593431,-65.2812689631459,
17.));
#16370=CARTESIAN_POINT('Ctrl Pts',(-207.725769513995,-65.2503238068458,
17.));
#16371=CARTESIAN_POINT('Ctrl Pts',(-207.725004679199,-65.2193479400861,
17.));
#16372=CARTESIAN_POINT('Ctrl Pts',(-207.723716132524,-65.188356011546,17.));
#16373=CARTESIAN_POINT('Ctrl Pts',(-207.723127462139,-65.1741974010323,
17.));
#16374=CARTESIAN_POINT('Ctrl Pts',(-207.722429402964,-65.1600353565386,
17.));
#16375=CARTESIAN_POINT('Ctrl Pts',(-207.721623066916,-65.1458857972683,
17.));
#16376=CARTESIAN_POINT('Ctrl Pts',(-207.716331511517,-65.0530297517173,
17.));
#16377=CARTESIAN_POINT('Ctrl Pts',(-207.706375521326,-64.9605544163374,
17.));
#16378=CARTESIAN_POINT('Ctrl Pts',(-207.69188291931,-64.8688309918216,17.));
#16379=CARTESIAN_POINT('Ctrl Pts',(-207.677420951151,-64.7773014484522,
17.));
#16380=CARTESIAN_POINT('Ctrl Pts',(-207.658441112453,-64.6865196943256,
17.));
#16381=CARTESIAN_POINT('Ctrl Pts',(-207.635021694811,-64.5968715427646,
17.));
#16382=CARTESIAN_POINT('Ctrl Pts',(-207.611997353704,-64.508735720912,17.));
#16383=CARTESIAN_POINT('Ctrl Pts',(-207.58468148308,-64.4216947907291,17.));
#16384=CARTESIAN_POINT('Ctrl Pts',(-207.553108101053,-64.3361444936322,
17.));
#16385=CARTESIAN_POINT('Ctrl Pts',(-207.536805168121,-64.2919705513309,
17.));
#16386=CARTESIAN_POINT('Ctrl Pts',(-207.519366487178,-64.2481945888456,
17.));
#16387=CARTESIAN_POINT('Ctrl Pts',(-207.500793029987,-64.2048752352537,
17.));
#16388=CARTESIAN_POINT('Ctrl Pts',(-207.494982654184,-64.191323545803,17.));
#16389=CARTESIAN_POINT('Ctrl Pts',(-207.489060435718,-64.1778148479559,
17.));
#16390=CARTESIAN_POINT('Ctrl Pts',(-207.483028790468,-64.1643564201991,
17.));
#16391=CARTESIAN_POINT('Ctrl Pts',(-207.44648471981,-64.0828155280312,17.));
#16392=CARTESIAN_POINT('Ctrl Pts',(-207.406050937059,-64.003390750436,17.));
#16393=CARTESIAN_POINT('Ctrl Pts',(-207.36180715762,-63.9264273776788,17.));
#16394=CARTESIAN_POINT('Ctrl Pts',(-207.318274262746,-63.8507006098065,
17.));
#16395=CARTESIAN_POINT('Ctrl Pts',(-207.271052355616,-63.7773560957185,
17.));
#16396=CARTESIAN_POINT('Ctrl Pts',(-207.22018022953,-63.7067557020002,17.));
#16397=CARTESIAN_POINT('Ctrl Pts',(-207.170937081922,-63.6384160064454,
17.));
#16398=CARTESIAN_POINT('Ctrl Pts',(-207.118273277825,-63.5726470624006,
17.));
#16399=CARTESIAN_POINT('Ctrl Pts',(-207.062195778224,-63.5098162258635,
17.));
#16400=CARTESIAN_POINT('Ctrl Pts',(-207.027350701924,-63.470774804462,17.));
#16401=CARTESIAN_POINT('Ctrl Pts',(-206.99118704962,-63.4328686004809,17.));
#16402=CARTESIAN_POINT('Ctrl Pts',(-206.953701849393,-63.3961948658342,
17.));
#16403=CARTESIAN_POINT('Ctrl Pts',(-206.941653045689,-63.3844068901223,
17.));
#16404=CARTESIAN_POINT('Ctrl Pts',(-206.929467677439,-63.372746308816,17.));
#16405=CARTESIAN_POINT('Ctrl Pts',(-206.917148223239,-63.3612143401441,
17.));
#16406=CARTESIAN_POINT('Origin',(-205.,-65.,-2.20842344717744));
#16407=CARTESIAN_POINT('Ctrl Pts',(-201.923731533573,-64.9977249101301,
0.291576552822544));
#16408=CARTESIAN_POINT('Ctrl Pts',(-201.922495961988,-64.8497482855437,
0.299259877064294));
#16409=CARTESIAN_POINT('Ctrl Pts',(-201.999549636482,-63.6828739087284,
0.359912640907479));
#16410=CARTESIAN_POINT('Ctrl Pts',(-203.493276918295,-61.6929032503864,
0.473534844352099));
#16411=CARTESIAN_POINT('Ctrl Pts',(-206.963857847912,-61.9425259124891,
0.632443163156407));
#16412=CARTESIAN_POINT('Ctrl Pts',(-208.633920228955,-64.9948075983619,
0.791351481960713));
#16413=CARTESIAN_POINT('Ctrl Pts',(-206.972481892344,-68.0520434541846,
0.950259800765019));
#16414=CARTESIAN_POINT('Ctrl Pts',(-203.502676360176,-68.3111058299649,
1.10916811956933));
#16415=CARTESIAN_POINT('Ctrl Pts',(-202.001256755867,-66.3232551853252,
1.22294037025517));
#16416=CARTESIAN_POINT('Ctrl Pts',(-201.922527589981,-65.1532534982625,
1.28374318133957));
#16417=CARTESIAN_POINT('Ctrl Pts',(-201.92380386931,-65.0023470817023,1.29157655282254));
#16418=CARTESIAN_POINT('Ctrl Pts',(-201.92961158086,-65.0031570762977,0.208423447177454));
#16419=CARTESIAN_POINT('Ctrl Pts',(-201.934956999492,-64.2978727303493,
0.24488784398784));
#16420=CARTESIAN_POINT('Ctrl Pts',(-202.525030743872,-62.5576537690219,
0.334321680399662));
#16421=CARTESIAN_POINT('Ctrl Pts',(-205.417645988708,-61.3907533400893,
0.47672495641292));
#16422=CARTESIAN_POINT('Ctrl Pts',(-208.260115801475,-63.3950087136501,
0.635633275217226));
#16423=CARTESIAN_POINT('Ctrl Pts',(-208.114970263096,-66.8719143799143,
0.794541594021533));
#16424=CARTESIAN_POINT('Ctrl Pts',(-205.113461147179,-68.6320808995075,
0.95344991282584));
#16425=CARTESIAN_POINT('Ctrl Pts',(-202.417561254516,-67.269564439631,1.09141053054448));
#16426=CARTESIAN_POINT('Ctrl Pts',(-201.933595089404,-65.6186981664531,
1.17640170866168));
#16427=CARTESIAN_POINT('Ctrl Pts',(-201.930556952874,-64.9983469618497,
1.20842344717745));
#16428=CARTESIAN_POINT('Ctrl Pts',(-206.913465996665,-63.364012796625,-1.94289029309402E-15));
#16429=CARTESIAN_POINT('Ctrl Pts',(-207.457950030113,-64.0008464354095,
0.0529694396014337));
#16430=CARTESIAN_POINT('Ctrl Pts',(-207.85066103992,-65.8508593102597,0.158908318804304));
#16431=CARTESIAN_POINT('Ctrl Pts',(-205.826538448717,-67.8612078721254,
0.317816637608612));
#16432=CARTESIAN_POINT('Ctrl Pts',(-203.043492499314,-67.2425410520485,
0.476724956412918));
#16433=CARTESIAN_POINT('Ctrl Pts',(-202.054683509666,-64.5708016763166,
0.635633275217225));
#16434=CARTESIAN_POINT('Ctrl Pts',(-203.765845011162,-62.291161195005,0.794541594021531));
#16435=CARTESIAN_POINT('Ctrl Pts',(-206.608593503211,-62.495626804845,0.953449912825838));
#16436=CARTESIAN_POINT('Ctrl Pts',(-207.97653950753,-64.9957469103226,1.11235823163015));
#16437=CARTESIAN_POINT('Ctrl Pts',(-206.615657447202,-67.4999249701999,
1.27126655043445));
#16438=CARTESIAN_POINT('Ctrl Pts',(-203.773544082233,-67.7121226376889,
1.43017486923876));
#16439=CARTESIAN_POINT('Ctrl Pts',(-202.055838893905,-65.4379140446217,
1.58908318804307));
#16440=CARTESIAN_POINT('Ctrl Pts',(-203.037304253044,-62.7622125536136,
1.74799150684737));
#16441=CARTESIAN_POINT('Ctrl Pts',(-205.818148811342,-62.1380984208763,
1.90689982565168));
#16442=CARTESIAN_POINT('Ctrl Pts',(-207.848922870067,-64.1377393756635,
2.06580814445599));
#16443=CARTESIAN_POINT('Ctrl Pts',(-207.267836678543,-66.9278933189866,
2.22471646326029));
#16444=CARTESIAN_POINT('Ctrl Pts',(-204.607622975304,-67.9505752021356,
2.3836247820646));
#16445=CARTESIAN_POINT('Ctrl Pts',(-202.307136236037,-66.2682032099886,
2.5425331008689));
#16446=CARTESIAN_POINT('Ctrl Pts',(-202.475436852696,-63.4231564503584,
2.70144141967321));
#16447=CARTESIAN_POINT('Ctrl Pts',(-204.958228768284,-62.0237423490828,
2.86034973847752));
#16448=CARTESIAN_POINT('Ctrl Pts',(-207.479316071554,-63.3529279407582,
3.01925805728183));
#16449=CARTESIAN_POINT('Ctrl Pts',(-207.727394116418,-66.1921308147553,
3.17816637608613));
#16450=CARTESIAN_POINT('Ctrl Pts',(-205.475027716348,-67.9384014686786,
3.33707469489044));
#16451=CARTESIAN_POINT('Ctrl Pts',(-202.787161216442,-66.9907785044862,
3.49598301369474));
#16452=CARTESIAN_POINT('Ctrl Pts',(-202.128000580265,-64.2180320547611,
3.65489133249906));
#16453=CARTESIAN_POINT('Ctrl Pts',(-204.101856912646,-62.162185078862,3.81379965130335));
#16454=CARTESIAN_POINT('Ctrl Pts',(-206.899120789014,-62.7080151042509,
3.97270797010767));
#16455=CARTESIAN_POINT('Ctrl Pts',(-207.955291952161,-65.3551112653809,
4.13161628891197));
#16456=CARTESIAN_POINT('Ctrl Pts',(-206.302084484222,-67.6766453872404,
4.29052460771628));
#16457=CARTESIAN_POINT('Ctrl Pts',(-203.455140514293,-67.5442609344747,
4.44943292652058));
#16458=CARTESIAN_POINT('Ctrl Pts',(-202.024506454277,-65.07932649362,4.60834124532489));
#16459=CARTESIAN_POINT('Ctrl Pts',(-203.321771620508,-62.5416664100502,
4.7672495641292));
#16460=CARTESIAN_POINT('Ctrl Pts',(-206.157617807844,-62.2577790854505,
4.92615788293351));
#16461=CARTESIAN_POINT('Ctrl Pts',(-207.932172927404,-64.4879292460782,
5.08506620173781));
#16462=CARTESIAN_POINT('Ctrl Pts',(-207.018544679411,-67.1875401505902,
5.24397452054212));
#16463=CARTESIAN_POINT('Ctrl Pts',(-204.25433723019,-67.8816386947262,5.40288283934643));
#16464=CARTESIAN_POINT('Ctrl Pts',(-202.173745074213,-65.9338830910165,
5.56179115815073));
#16465=CARTESIAN_POINT('Ctrl Pts',(-202.68423184573,-63.1299539072815,5.72069947695504));
#16466=CARTESIAN_POINT('Ctrl Pts',(-205.31778897822,-62.040462080232,5.87960779575935));
#16467=CARTESIAN_POINT('Ctrl Pts',(-207.66000072734,-63.6642415398826,6.03851611456366));
#16468=CARTESIAN_POINT('Ctrl Pts',(-207.563553539912,-66.5126294262725,
6.19742443336796));
#16469=CARTESIAN_POINT('Ctrl Pts',(-205.116869119401,-67.9742555610023,
6.35633275217227));
#16470=CARTESIAN_POINT('Ctrl Pts',(-202.563040396445,-66.7091174400446,
6.51524107097658));
#16471=CARTESIAN_POINT('Ctrl Pts',(-202.243389000634,-63.8770795525063,
6.67414938978088));
#16472=CARTESIAN_POINT('Ctrl Pts',(-204.450967758971,-62.0745225805805,
6.83305770858518));
#16473=CARTESIAN_POINT('Ctrl Pts',(-207.161893139463,-62.9540106093222,
6.99196602738949));
#16474=CARTESIAN_POINT('Ctrl Pts',(-207.890819052728,-65.709238843837,7.15087434619381));
#16475=CARTESIAN_POINT('Ctrl Pts',(-205.969474368539,-67.8142448333378,
7.3097826649981));
#16476=CARTESIAN_POINT('Ctrl Pts',(-203.159326418888,-67.3391826138673,
7.46869098380242));
#16477=CARTESIAN_POINT('Ctrl Pts',(-202.036687435572,-64.7195839185636,
7.62759930260671));
#16478=CARTESIAN_POINT('Ctrl Pts',(-203.630780290992,-62.3570675525683,
7.78650762141104));
#16479=CARTESIAN_POINT('Ctrl Pts',(-206.480158472145,-62.4175621148688,
7.94541594021532));
#16480=CARTESIAN_POINT('Ctrl Pts',(-207.97254390946,-64.8456068668834,8.10432425901965));
#16481=CARTESIAN_POINT('Ctrl Pts',(-206.739734314091,-67.415197517719,8.26323257782394));
#16482=CARTESIAN_POINT('Ctrl Pts',(-203.911955744214,-67.7705620784733,
8.42214089662826));
#16483=CARTESIAN_POINT('Ctrl Pts',(-202.081683987196,-65.5859062916828,
8.58104921543255));
#16484=CARTESIAN_POINT('Ctrl Pts',(-202.926891733301,-62.8640981652309,
8.73995753423687));
#16485=CARTESIAN_POINT('Ctrl Pts',(-205.672701967614,-62.1004609683623,
8.89886585304117));
#16486=CARTESIAN_POINT('Ctrl Pts',(-207.801786556669,-63.9950887481507,
9.05777417184549));
#16487=CARTESIAN_POINT('Ctrl Pts',(-207.362224545558,-66.8110079319493,
9.21668249064978));
#16488=CARTESIAN_POINT('Ctrl Pts',(-204.757001473176,-67.966615284998,9.37559080945409));
#16489=CARTESIAN_POINT('Ctrl Pts',(-202.374556734241,-66.4024629020062,
9.53449912825839));
#16490=CARTESIAN_POINT('Ctrl Pts',(-202.399089037318,-63.5525482054929,
9.69340744706271));
#16491=CARTESIAN_POINT('Ctrl Pts',(-204.808107441137,-62.0296411363144,
9.85231576586701));
#16492=CARTESIAN_POINT('Ctrl Pts',(-207.393050798179,-63.2299258742758,
10.0112240846713));
#16493=CARTESIAN_POINT('Ctrl Pts',(-207.784071930084,-66.0529947869487,
10.1701324034756));
#16494=CARTESIAN_POINT('Ctrl Pts',(-205.622687033484,-67.910689848052,10.3290407222799));
#16495=CARTESIAN_POINT('Ctrl Pts',(-202.890429624231,-67.0998969886399,
10.4879490410842));
#16496=CARTESIAN_POINT('Ctrl Pts',(-202.09220275725,-64.3639420401572,10.6468573598885));
#16497=CARTESIAN_POINT('Ctrl Pts',(-203.959811902574,-62.2111179201701,
10.8057656786929));
#16498=CARTESIAN_POINT('Ctrl Pts',(-206.781053869651,-62.6151097202126,
10.9646739974972));
#16499=CARTESIAN_POINT('Ctrl Pts',(-207.969445555503,-65.2055422733386,
11.1235823163015));
#16500=CARTESIAN_POINT('Ctrl Pts',(-206.435482744948,-67.6075359675713,
11.2824906351058));
#16501=CARTESIAN_POINT('Ctrl Pts',(-203.58548539792,-67.618969830625,11.4413989539101));
#16502=CARTESIAN_POINT('Ctrl Pts',(-202.032299228341,-65.229361424646,11.6003072727144));
#16503=CARTESIAN_POINT('Ctrl Pts',(-203.199867956841,-62.6294770280768,
11.7592155915187));
#16504=CARTESIAN_POINT('Ctrl Pts',(-206.017777622806,-62.2028615973215,
11.918123910323));
#16505=CARTESIAN_POINT('Ctrl Pts',(-207.902600139672,-64.3406313911045,
12.0770322291273));
#16506=CARTESIAN_POINT('Ctrl Pts',(-207.126351290249,-67.0829029558956,
12.2359405479316));
#16507=CARTESIAN_POINT('Ctrl Pts',(-204.400687343713,-67.9155923708988,
12.3948488667359));
#16508=CARTESIAN_POINT('Ctrl Pts',(-202.22446654207,-66.0752992872318,12.5537571855402));
#16509=CARTESIAN_POINT('Ctrl Pts',(-202.592823793087,-63.2491838354354,
12.7126655043445));
#16510=CARTESIAN_POINT('Ctrl Pts',(-205.168053286105,-62.0281970747873,
12.8715738231488));
#16511=CARTESIAN_POINT('Ctrl Pts',(-207.589213404689,-63.5317260207767,
13.0304821419532));
#16512=CARTESIAN_POINT('Ctrl Pts',(-207.636611613018,-66.3813521402626,
13.1893904607575));
#16513=CARTESIAN_POINT('Ctrl Pts',(-205.266793763269,-67.9645700567683,
13.3482987795618));
#16514=CARTESIAN_POINT('Ctrl Pts',(-202.652382373513,-66.8299032793574,
13.5072070983661));
#16515=CARTESIAN_POINT('Ctrl Pts',(-202.190240584349,-64.0176016284133,
13.6661154171704));
#16516=CARTESIAN_POINT('Ctrl Pts',(-204.304054824455,-62.1059518233833,
13.8250237359747));
#16517=CARTESIAN_POINT('Ctrl Pts',(-207.055903820797,-62.8475330427476,
13.983932054779));
#16518=CARTESIAN_POINT('Ctrl Pts',(-207.922923177315,-65.5624719062102,
14.1428403735833));
#16519=CARTESIAN_POINT('Ctrl Pts',(-206.110239224163,-67.7617428222285,
14.3017486923876));
#16520=CARTESIAN_POINT('Ctrl Pts',(-203.279700379008,-67.4290787666223,
14.4606570111919));
#16521=CARTESIAN_POINT('Ctrl Pts',(-202.026312958194,-64.8694624875084,
14.6195653299962));
#16522=CARTESIAN_POINT('Ctrl Pts',(-203.499168664916,-62.4295214576422,
14.7784736488005));
#16523=CARTESIAN_POINT('Ctrl Pts',(-206.34796959245,-62.3461665970152,14.9373819676048));
#16524=CARTESIAN_POINT('Ctrl Pts',(-207.960967419167,-64.6958161862147,
15.0962902864091));
#16525=CARTESIAN_POINT('Ctrl Pts',(-206.85938267811,-67.3243388221629,15.2551986052134));
#16526=CARTESIAN_POINT('Ctrl Pts',(-204.053138186676,-67.8219321098425,
15.4141069240177));
#16527=CARTESIAN_POINT('Ctrl Pts',(-202.114962920394,-65.7324126566496,
15.5730152428221));
#16528=CARTESIAN_POINT('Ctrl Pts',(-202.821763790211,-62.9714191306523,
15.7319235616264));
#16529=CARTESIAN_POINT('Ctrl Pts',(-205.525534122556,-62.0702189149839,
15.8908318804307));
#16530=CARTESIAN_POINT('Ctrl Pts',(-207.747527714867,-63.8549824021587,
16.049740199235));
#16531=CARTESIAN_POINT('Ctrl Pts',(-207.450562878104,-66.6895405023604,
16.2086485180393));
#16532=CARTESIAN_POINT('Ctrl Pts',(-204.907064112986,-67.975032954454,16.3675568368436));
#16533=CARTESIAN_POINT('Ctrl Pts',(-202.448531736689,-66.5332827231908,
16.5264651556479));
#16534=CARTESIAN_POINT('Ctrl Pts',(-202.329643199581,-63.6853536643865,
16.6853734744522));
#16535=CARTESIAN_POINT('Ctrl Pts',(-204.657906690574,-62.0436704956976,
16.8442817932565));
#16536=CARTESIAN_POINT('Ctrl Pts',(-207.301858842744,-63.1102587047955,
17.0031901120608));
#16537=CARTESIAN_POINT('Ctrl Pts',(-207.831197343881,-65.9135379195059,
17.1620984308651));
#16538=CARTESIAN_POINT('Ctrl Pts',(-206.459639356019,-67.2156893163364,
17.268037310068));
#16539=CARTESIAN_POINT('Ctrl Pts',(-205.650199997975,-67.4320868020351,
17.3210067496694));
#16540=CARTESIAN_POINT('Ctrl Pts',(-207.054331550342,-63.2435746787731,
-0.107002249889813));
#16541=CARTESIAN_POINT('Ctrl Pts',(-207.63889941333,-63.9272907410153,-0.054032810288377));
#16542=CARTESIAN_POINT('Ctrl Pts',(-208.060521025117,-65.9134978771587,
0.051906068914494));
#16543=CARTESIAN_POINT('Ctrl Pts',(-205.887386562254,-68.0718442940919,
0.210814387718801));
#16544=CARTESIAN_POINT('Ctrl Pts',(-202.899458315881,-67.4076324555492,
0.369722706523107));
#16545=CARTESIAN_POINT('Ctrl Pts',(-201.837855178832,-64.5392049509981,
0.528631025327414));
#16546=CARTESIAN_POINT('Ctrl Pts',(-203.674988980207,-62.0917418801321,
0.687539344131721));
#16547=CARTESIAN_POINT('Ctrl Pts',(-206.727014951444,-62.3112598407265,
0.846447662936028));
#16548=CARTESIAN_POINT('Ctrl Pts',(-208.195666414672,-64.9954338063356,
1.00535598174033));
#16549=CARTESIAN_POINT('Ctrl Pts',(-206.734598928916,-67.6839644648615,
1.16426430054464));
#16550=CARTESIAN_POINT('Ctrl Pts',(-203.683254841548,-67.9117837017809,
1.32317261934895));
#16551=CARTESIAN_POINT('Ctrl Pts',(-201.839095620156,-65.4701524039476,
1.48208093815325));
#16552=CARTESIAN_POINT('Ctrl Pts',(-202.892814503252,-62.5974711010892,
1.64098925695756));
#16553=CARTESIAN_POINT('Ctrl Pts',(-205.878379296494,-61.9274109295829,
1.79989757576187));
#16554=CARTESIAN_POINT('Ctrl Pts',(-208.058654894662,-64.0742614667419,
1.95880589456618));
#16555=CARTESIAN_POINT('Ctrl Pts',(-207.434790295659,-67.0698209833833,
2.11771421337048));
#16556=CARTESIAN_POINT('Ctrl Pts',(-204.578736960642,-68.1677906688536,
2.27662253217479));
#16557=CARTESIAN_POINT('Ctrl Pts',(-202.108892971851,-66.3615658031371,
2.4355308509791));
#16558=CARTESIAN_POINT('Ctrl Pts',(-202.289583544533,-63.3070723704377,
2.5944391697834));
#16559=CARTESIAN_POINT('Ctrl Pts',(-204.955153653443,-61.8046361916634,
2.75334748858771));
#16560=CARTESIAN_POINT('Ctrl Pts',(-207.661838380165,-63.2316737779064,
2.91225580739202));
#16561=CARTESIAN_POINT('Ctrl Pts',(-207.928179436342,-66.2798931097576,
3.07116412619632));
#16562=CARTESIAN_POINT('Ctrl Pts',(-205.50999831023,-68.1547207293982,3.23007244500063));
#16563=CARTESIAN_POINT('Ctrl Pts',(-202.624256434759,-67.1373356509271,
3.38898076380493));
#16564=CARTESIAN_POINT('Ctrl Pts',(-201.916569706068,-64.160465132874,3.54788908260924));
#16565=CARTESIAN_POINT('Ctrl Pts',(-204.035737408301,-61.9532707993317,
3.70679740141355));
#16566=CARTESIAN_POINT('Ctrl Pts',(-207.038930277089,-62.5392837435045,
3.86570572021786));
#16567=CARTESIAN_POINT('Ctrl Pts',(-208.172854656617,-65.3812538491018,
4.02461403902216));
#16568=CARTESIAN_POINT('Ctrl Pts',(-206.397941349264,-67.8736946868505,
4.18352235782647));
#16569=CARTESIAN_POINT('Ctrl Pts',(-203.341411037424,-67.7315643544771,
4.34243067663077));
#16570=CARTESIAN_POINT('Ctrl Pts',(-201.80545654876,-65.085166352005,4.50133899543508));
#16571=CARTESIAN_POINT('Ctrl Pts',(-203.198223791445,-62.3606887899229,
4.66024731423939));
#16572=CARTESIAN_POINT('Ctrl Pts',(-206.242839324052,-62.0559022461933,
4.8191556330437));
#16573=CARTESIAN_POINT('Ctrl Pts',(-208.148033655327,-64.450231617587,4.978063951848));
#16574=CARTESIAN_POINT('Ctrl Pts',(-207.167145916319,-67.3485824973268,
5.13697227065231));
#16575=CARTESIAN_POINT('Ctrl Pts',(-204.199443022972,-68.0937791931397,
5.29588058945662));
#16576=CARTESIAN_POINT('Ctrl Pts',(-201.965681818504,-66.0026337032119,
5.45478890826092));
#16577=CARTESIAN_POINT('Ctrl Pts',(-202.513749608885,-62.9922848404093,
5.61369722706523));
#16578=CARTESIAN_POINT('Ctrl Pts',(-205.341183969533,-61.8225867961021,
5.77260554586953));
#16579=CARTESIAN_POINT('Ctrl Pts',(-207.855824680256,-63.5659056638381,
5.93151386467385));
#16580=CARTESIAN_POINT('Ctrl Pts',(-207.752277243082,-66.6239861903914,
6.09042218347815));
#16581=CARTESIAN_POINT('Ctrl Pts',(-205.125472791084,-68.1932143285518,
6.24933050228246));
#16582=CARTESIAN_POINT('Ctrl Pts',(-202.383636286604,-66.8349392601922,
6.40823882108676));
#16583=CARTESIAN_POINT('Ctrl Pts',(-202.040452792008,-63.7944123868251,
6.56714713989107));
#16584=CARTESIAN_POINT('Ctrl Pts',(-204.410549099453,-61.8591547626134,
6.72605545869538));
#16585=CARTESIAN_POINT('Ctrl Pts',(-207.321047404347,-62.8033889474597,
6.88496377749968));
#16586=CARTESIAN_POINT('Ctrl Pts',(-208.103635390804,-65.7614515942076,
7.04387209630399));
#16587=CARTESIAN_POINT('Ctrl Pts',(-206.040845139662,-68.0214239299728,
7.2027804151083));
#16588=CARTESIAN_POINT('Ctrl Pts',(-203.023819697789,-67.5113885765698,
7.36168873391261));
#16589=CARTESIAN_POINT('Ctrl Pts',(-201.818534269624,-64.6989402454383,
7.52059705271691));
#16590=CARTESIAN_POINT('Ctrl Pts',(-203.529981064483,-62.1625001324065,
7.67950537152122));
#16591=CARTESIAN_POINT('Ctrl Pts',(-206.589124789326,-62.227448183835,7.83841369032552));
#16592=CARTESIAN_POINT('Ctrl Pts',(-208.191376668634,-64.8342407520852,
7.99732200912984));
#16593=CARTESIAN_POINT('Ctrl Pts',(-206.867810087495,-67.5929995461668,
8.15623032793414));
#16594=CARTESIAN_POINT('Ctrl Pts',(-203.831856094268,-67.9745253377426,
8.31513864673845));
#16595=CARTESIAN_POINT('Ctrl Pts',(-201.866843377713,-65.6290395453307,
8.47404696554276));
#16596=CARTESIAN_POINT('Ctrl Pts',(-202.774273633827,-62.7068573284045,
8.63295528434705));
#16597=CARTESIAN_POINT('Ctrl Pts',(-205.722224945965,-61.8870026828157,
8.79186360315137));
#16598=CARTESIAN_POINT('Ctrl Pts',(-208.008048499801,-63.921109184294,8.95077192195566));
#16599=CARTESIAN_POINT('Ctrl Pts',(-207.536126809356,-66.944330727072,9.10968024075998));
#16600=CARTESIAN_POINT('Ctrl Pts',(-204.739112405858,-68.185011590653,9.26858855956428));
#16601=CARTESIAN_POINT('Ctrl Pts',(-202.181276832783,-66.5057094261393,
9.42749687836859));
#16602=CARTESIAN_POINT('Ctrl Pts',(-202.207615155126,-63.4459896887441,
9.5864051971729));
#16603=CARTESIAN_POINT('Ctrl Pts',(-204.793980693342,-61.8109692358563,
9.7453135159772));
#16604=CARTESIAN_POINT('Ctrl Pts',(-207.569222429266,-63.099616544398,9.90422183478152));
#16605=CARTESIAN_POINT('Ctrl Pts',(-207.989029757708,-66.1305141648425,
10.0631301535858));
#16606=CARTESIAN_POINT('Ctrl Pts',(-205.66852801205,-68.1249690344826,10.2220384723901));
#16607=CARTESIAN_POINT('Ctrl Pts',(-202.735127256945,-67.2544872204418,
10.3809467911944));
#16608=CARTESIAN_POINT('Ctrl Pts',(-201.878136518658,-64.3171167206374,
10.5398551099987));
#16609=CARTESIAN_POINT('Ctrl Pts',(-203.883235327643,-62.0058059789076,
10.698763428803));
#16610=CARTESIAN_POINT('Ctrl Pts',(-206.912171506397,-62.4395388502276,
10.8576717476073));
#16611=CARTESIAN_POINT('Ctrl Pts',(-208.188050220032,-65.2206738859141,
11.0165800664116));
#16612=CARTESIAN_POINT('Ctrl Pts',(-206.54116012412,-67.799497569421,11.175488385216));
#16613=CARTESIAN_POINT('Ctrl Pts',(-203.481351651642,-67.8117731706882,
11.3343967040203));
#16614=CARTESIAN_POINT('Ctrl Pts',(-201.813823011321,-65.2462465556759,
11.4933050228246));
#16615=CARTESIAN_POINT('Ctrl Pts',(-203.067345822979,-62.4549638506668,
11.6522133416289));
#16616=CARTESIAN_POINT('Ctrl Pts',(-206.092704383254,-61.9969418420234,
11.8111216604332));
#16617=CARTESIAN_POINT('Ctrl Pts',(-208.116283777892,-64.2920899880532,
11.9700299792375));
#16618=CARTESIAN_POINT('Ctrl Pts',(-207.28288903502,-67.2362421208711,12.1289382980418));
#16619=CARTESIAN_POINT('Ctrl Pts',(-204.356567140218,-68.130232471292,12.2878466168461));
#16620=CARTESIAN_POINT('Ctrl Pts',(-202.020137299752,-66.1544606779899,
12.4467549356504));
#16621=CARTESIAN_POINT('Ctrl Pts',(-202.415612277557,-63.1202922382824,
12.6056632544547));
#16622=CARTESIAN_POINT('Ctrl Pts',(-205.180425034146,-61.8094188653972,
12.764571573259));
#16623=CARTESIAN_POINT('Ctrl Pts',(-207.779826135971,-63.4236346162818,
12.9234798920633));
#16624=CARTESIAN_POINT('Ctrl Pts',(-207.830713705946,-66.483044532184,13.0823882108676));
#16625=CARTESIAN_POINT('Ctrl Pts',(-205.286434588476,-68.1828157967964,
13.241296529672));
#16626=CARTESIAN_POINT('Ctrl Pts',(-202.47955544199,-66.9646171123032,13.4002048484763));
#16627=CARTESIAN_POINT('Ctrl Pts',(-201.983391695226,-63.9452794179396,
13.5591131672806));
#16628=CARTESIAN_POINT('Ctrl Pts',(-204.252820727453,-61.8928977636416,
13.7180214860849));
#16629=CARTESIAN_POINT('Ctrl Pts',(-207.207255363249,-62.6890727146135,
13.8769298048892));
#16630=CARTESIAN_POINT('Ctrl Pts',(-208.138102957068,-65.6038799670978,
14.0358381236935));
#16631=CARTESIAN_POINT('Ctrl Pts',(-206.191972823453,-67.9650568254273,
14.1947464424978));
#16632=CARTESIAN_POINT('Ctrl Pts',(-203.153055348982,-67.607902704953,14.3536547613021));
#16633=CARTESIAN_POINT('Ctrl Pts',(-201.807396043895,-64.8598525759631,
14.5125630801064));
#16634=CARTESIAN_POINT('Ctrl Pts',(-203.388680452761,-62.2402879495917,
14.6714713989107));
#16635=CARTESIAN_POINT('Ctrl Pts',(-206.447204427723,-62.150796670228,14.830379717715));
#16636=CARTESIAN_POINT('Ctrl Pts',(-208.178947940194,-64.6734227799964,
14.9892880365193));
#16637=CARTESIAN_POINT('Ctrl Pts',(-206.996266725648,-67.4954520144994,
15.1481963553236));
#16638=CARTESIAN_POINT('Ctrl Pts',(-203.983432106807,-68.0296771284552,
15.3071046741279));
#16639=CARTESIAN_POINT('Ctrl Pts',(-201.902572239658,-65.7863314169405,
15.4660129929322));
#16640=CARTESIAN_POINT('Ctrl Pts',(-202.661406381056,-62.8220790494398,
15.6249213117365));
#16641=CARTESIAN_POINT('Ctrl Pts',(-205.564222897418,-61.8545342697314,
15.7838296305408));
#16642=CARTESIAN_POINT('Ctrl Pts',(-207.949795230189,-63.7706884883024,
15.9427379493452));
#16643=CARTESIAN_POINT('Ctrl Pts',(-207.63096843391,-66.8139211073671,16.1016462681495));
#16644=CARTESIAN_POINT('Ctrl Pts',(-204.900222358179,-68.1940489521602,
16.2605545869538));
#16645=CARTESIAN_POINT('Ctrl Pts',(-202.2606977275,-66.6461599418726,16.4194629057581));
#16646=CARTESIAN_POINT('Ctrl Pts',(-202.133056853201,-63.5885720208776,
16.5783712245624));
#16647=CARTESIAN_POINT('Ctrl Pts',(-204.632722462829,-61.8260314087208,
16.7372795433667));
#16648=CARTESIAN_POINT('Ctrl Pts',(-207.471317103792,-62.9711397163634,
16.896187862171));
#16649=CARTESIAN_POINT('Ctrl Pts',(-208.039624450561,-65.9807907607168,
17.0550961809753));
#16650=CARTESIAN_POINT('Ctrl Pts',(-206.56709509676,-67.3788039485619,17.1610350601782));
#16651=CARTESIAN_POINT('Ctrl Pts',(-205.698066426161,-67.6111321859386,
17.2140044997796));
#16652=CARTESIAN_POINT('Ctrl Pts',(-207.195197104019,-63.1231365609212,
-0.214004499779623));
#16653=CARTESIAN_POINT('Ctrl Pts',(-207.819848796546,-63.8537350466211,
-0.161035060178188));
#16654=CARTESIAN_POINT('Ctrl Pts',(-208.270381010313,-65.9761364440577,
-0.0550961809753165));
#16655=CARTESIAN_POINT('Ctrl Pts',(-205.948234675791,-68.2824807160583,
0.10381213782899));
#16656=CARTESIAN_POINT('Ctrl Pts',(-202.755424132447,-67.5727238590499,
0.262720456633297));
#16657=CARTESIAN_POINT('Ctrl Pts',(-201.621026847998,-64.5076082256796,
0.421628775437604));
#16658=CARTESIAN_POINT('Ctrl Pts',(-203.584132949251,-61.8923225652592,
0.58053709424191));
#16659=CARTESIAN_POINT('Ctrl Pts',(-206.845436399678,-62.1268928766078,
0.739445413046217));
#16660=CARTESIAN_POINT('Ctrl Pts',(-208.414793321813,-64.9951207023487,
0.898353731850525));
#16661=CARTESIAN_POINT('Ctrl Pts',(-206.85354041063,-67.8680039595231,1.05726205065483));
#16662=CARTESIAN_POINT('Ctrl Pts',(-203.592965600862,-68.1114447658729,
1.21617036945914));
#16663=CARTESIAN_POINT('Ctrl Pts',(-201.622352346407,-65.5023907632737,
1.37507868826344));
#16664=CARTESIAN_POINT('Ctrl Pts',(-202.74832475346,-62.4327296485647,1.53398700706775));
#16665=CARTESIAN_POINT('Ctrl Pts',(-205.938609781645,-61.7167234382895,
1.69289532587206));
#16666=CARTESIAN_POINT('Ctrl Pts',(-208.268386919257,-64.0107835578202,
1.85180364467636));
#16667=CARTESIAN_POINT('Ctrl Pts',(-207.601743912775,-67.2117486477801,
2.01071196348067));
#16668=CARTESIAN_POINT('Ctrl Pts',(-204.549850945981,-68.3850061355715,
2.16962028228498));
#16669=CARTESIAN_POINT('Ctrl Pts',(-201.910649707665,-66.4549283962856,
2.32852860108928));
#16670=CARTESIAN_POINT('Ctrl Pts',(-202.10373023637,-63.190988290517,2.48743691989359));
#16671=CARTESIAN_POINT('Ctrl Pts',(-204.952078538602,-61.585530034244,2.6463452386979));
#16672=CARTESIAN_POINT('Ctrl Pts',(-207.844360688776,-63.1104196150545,
2.8052535575022));
#16673=CARTESIAN_POINT('Ctrl Pts',(-208.128964756266,-66.3676554047598,
2.96416187630651));
#16674=CARTESIAN_POINT('Ctrl Pts',(-205.544968904111,-68.3710399901179,
3.12307019511081));
#16675=CARTESIAN_POINT('Ctrl Pts',(-202.461351653077,-67.2838927973679,
3.28197851391513));
#16676=CARTESIAN_POINT('Ctrl Pts',(-201.705138831871,-64.1028982109869,
3.44088683271943));
#16677=CARTESIAN_POINT('Ctrl Pts',(-203.969617903956,-61.7443565198013,
3.59979515152374));
#16678=CARTESIAN_POINT('Ctrl Pts',(-207.178739765165,-62.3705523827582,
3.75870347032805));
#16679=CARTESIAN_POINT('Ctrl Pts',(-208.390417361073,-65.4073964328226,
3.91761178913235));
#16680=CARTESIAN_POINT('Ctrl Pts',(-206.493798214305,-68.0707439864606,
4.07652010793666));
#16681=CARTESIAN_POINT('Ctrl Pts',(-203.227681560555,-67.9188677744795,
4.23542842674097));
#16682=CARTESIAN_POINT('Ctrl Pts',(-201.586406643242,-65.0910062103899,
4.39433674554527));
#16683=CARTESIAN_POINT('Ctrl Pts',(-203.074675962382,-62.1797111697955,
4.55324506434958));
#16684=CARTESIAN_POINT('Ctrl Pts',(-206.32806084026,-61.8540254069362,4.71215338315389));
#16685=CARTESIAN_POINT('Ctrl Pts',(-208.363894383249,-64.4125339890956,
4.87106170195819));
#16686=CARTESIAN_POINT('Ctrl Pts',(-207.315747153228,-67.5096248440634,
5.0299700207625));
#16687=CARTESIAN_POINT('Ctrl Pts',(-204.144548815754,-68.3059196915532,
5.1888783395668));
#16688=CARTESIAN_POINT('Ctrl Pts',(-201.757618562796,-66.0713843154072,
5.34778665837111));
#16689=CARTESIAN_POINT('Ctrl Pts',(-202.34326737204,-62.8546157735372,5.50669497717542));
#16690=CARTESIAN_POINT('Ctrl Pts',(-205.364578960846,-61.6047115119722,
5.66560329597973));
#16691=CARTESIAN_POINT('Ctrl Pts',(-208.051648633173,-63.4675697877938,
5.82451161478403));
#16692=CARTESIAN_POINT('Ctrl Pts',(-207.941000946252,-66.7353429545102,
5.98341993358834));
#16693=CARTESIAN_POINT('Ctrl Pts',(-205.134076462768,-68.4121730961013,
6.14232825239265));
#16694=CARTESIAN_POINT('Ctrl Pts',(-202.204232176763,-66.9607610803398,
6.30123657119695));
#16695=CARTESIAN_POINT('Ctrl Pts',(-201.837516583383,-63.7117452211441,
6.46014489000126));
#16696=CARTESIAN_POINT('Ctrl Pts',(-204.370130439934,-61.6437869446461,
6.61905320880556));
#16697=CARTESIAN_POINT('Ctrl Pts',(-207.480201669232,-62.6527672855972,
6.77796152760987));
#16698=CARTESIAN_POINT('Ctrl Pts',(-208.31645172888,-65.813664344578,6.93686984641418));
#16699=CARTESIAN_POINT('Ctrl Pts',(-206.112215910785,-68.2286030266078,
7.09577816521849));
#16700=CARTESIAN_POINT('Ctrl Pts',(-202.888312976691,-67.6835945392722,
7.25468648402279));
#16701=CARTESIAN_POINT('Ctrl Pts',(-201.600381103676,-64.678296572313,7.4135948028271));
#16702=CARTESIAN_POINT('Ctrl Pts',(-203.429181837975,-61.9679327122447,
7.5725031216314));
#16703=CARTESIAN_POINT('Ctrl Pts',(-206.698091106507,-62.0373342528012,
7.73141144043571));
#16704=CARTESIAN_POINT('Ctrl Pts',(-208.410209427808,-64.8228746372871,
7.89031975924003));
#16705=CARTESIAN_POINT('Ctrl Pts',(-206.995885860899,-67.7708015746146,
8.04922807804432));
#16706=CARTESIAN_POINT('Ctrl Pts',(-203.751756444322,-68.1784885970118,
8.20813639684863));
#16707=CARTESIAN_POINT('Ctrl Pts',(-201.65200276823,-65.6721727989785,8.36704471565294));
#16708=CARTESIAN_POINT('Ctrl Pts',(-202.621655534352,-62.5496164915781,
8.52595303445724));
#16709=CARTESIAN_POINT('Ctrl Pts',(-205.771747924315,-61.6735443972691,
8.68486135326156));
#16710=CARTESIAN_POINT('Ctrl Pts',(-208.214310442934,-63.8471296204372,
8.84376967206585));
#16711=CARTESIAN_POINT('Ctrl Pts',(-207.710029073154,-67.0776535221947,
9.00267799087017));
#16712=CARTESIAN_POINT('Ctrl Pts',(-204.721223338541,-68.4034078963079,
9.16158630967447));
#16713=CARTESIAN_POINT('Ctrl Pts',(-201.987996931325,-66.6089559502724,
9.32049462847878));
#16714=CARTESIAN_POINT('Ctrl Pts',(-202.016141272935,-63.3394311719952,
9.47940294728309));
#16715=CARTESIAN_POINT('Ctrl Pts',(-204.779853945546,-61.5922973353983,
9.63831126608739));
#16716=CARTESIAN_POINT('Ctrl Pts',(-207.745394060354,-62.9693072145201,
9.7972195848917));
#16717=CARTESIAN_POINT('Ctrl Pts',(-208.193987585331,-66.2080335427364,
9.95612790369601));
#16718=CARTESIAN_POINT('Ctrl Pts',(-205.714368990616,-68.3392482209132,
10.1150362225003));
#16719=CARTESIAN_POINT('Ctrl Pts',(-202.579824889659,-67.4090774522437,
10.2739445413046));
#16720=CARTESIAN_POINT('Ctrl Pts',(-201.664070280065,-64.2702914011178,
10.4328528601089));
#16721=CARTESIAN_POINT('Ctrl Pts',(-203.806658752712,-61.800494037645,10.5917611789132));
#16722=CARTESIAN_POINT('Ctrl Pts',(-207.043289143143,-62.2639679802425,
10.7506694977175));
#16723=CARTESIAN_POINT('Ctrl Pts',(-208.406654884562,-65.2358054984896,
10.9095778165218));
#16724=CARTESIAN_POINT('Ctrl Pts',(-206.646837503291,-67.9914591712706,
11.0684861353262));
#16725=CARTESIAN_POINT('Ctrl Pts',(-203.377217905366,-68.0045765107515,
11.2273944541305));
#16726=CARTESIAN_POINT('Ctrl Pts',(-201.595346794301,-65.2631316867057,
11.3863027729348));
#16727=CARTESIAN_POINT('Ctrl Pts',(-202.934823689116,-62.2804506732568,
11.5452110917391));
#16728=CARTESIAN_POINT('Ctrl Pts',(-206.167631143701,-61.7910220867251,
11.7041194105434));
#16729=CARTESIAN_POINT('Ctrl Pts',(-208.329967416112,-64.2435485850018,
11.8630277293477));
#16730=CARTESIAN_POINT('Ctrl Pts',(-207.43942677979,-67.3895812858467,12.021936048152));
#16731=CARTESIAN_POINT('Ctrl Pts',(-204.312446936723,-68.3448725716852,
12.1808443669563));
#16732=CARTESIAN_POINT('Ctrl Pts',(-201.815808057434,-66.233622068748,12.3397526857606));
#16733=CARTESIAN_POINT('Ctrl Pts',(-202.238400762026,-62.9914006411294,
12.4986610045649));
#16734=CARTESIAN_POINT('Ctrl Pts',(-205.192796782186,-61.5906406560071,
12.6575693233692));
#16735=CARTESIAN_POINT('Ctrl Pts',(-207.970438867253,-63.3155432117869,
12.8164776421735));
#16736=CARTESIAN_POINT('Ctrl Pts',(-208.024815798874,-66.5847369241054,
12.9753859609778));
#16737=CARTESIAN_POINT('Ctrl Pts',(-205.306075413683,-68.4010615368247,
13.1342942797821));
#16738=CARTESIAN_POINT('Ctrl Pts',(-202.306728510468,-67.099330945249,13.2932025985865));
#16739=CARTESIAN_POINT('Ctrl Pts',(-201.776542806102,-63.8729572074659,
13.4521109173907));
#16740=CARTESIAN_POINT('Ctrl Pts',(-204.201586630452,-61.6798437039,13.6110192361951));
#16741=CARTESIAN_POINT('Ctrl Pts',(-207.3586069057,-62.5306123864796,13.7699275549994));
#16742=CARTESIAN_POINT('Ctrl Pts',(-208.353282736821,-65.6452880279853,
13.9288358738037));
#16743=CARTESIAN_POINT('Ctrl Pts',(-206.273706422742,-68.1683708286262,
14.087744192608));
#16744=CARTESIAN_POINT('Ctrl Pts',(-203.026410318955,-67.7867266432836,
14.2466525114123));
#16745=CARTESIAN_POINT('Ctrl Pts',(-201.588479129595,-64.8502426644178,
14.4055608302166));
#16746=CARTESIAN_POINT('Ctrl Pts',(-203.278192240605,-62.0510544415413,
14.5644691490209));
#16747=CARTESIAN_POINT('Ctrl Pts',(-206.546439262996,-61.9554267434409,
14.7233774678252));
#16748=CARTESIAN_POINT('Ctrl Pts',(-208.396928461221,-64.6510293737779,
14.8822857866295));
#16749=CARTESIAN_POINT('Ctrl Pts',(-207.133150773185,-67.6665652068362,
15.0411941054338));
#16750=CARTESIAN_POINT('Ctrl Pts',(-203.913726026938,-68.2374221470678,
15.2001024242381));
#16751=CARTESIAN_POINT('Ctrl Pts',(-201.690181558921,-65.8402501772315,
15.3590107430424));
#16752=CARTESIAN_POINT('Ctrl Pts',(-202.501048971901,-62.6727389682273,
15.5179190618468));
#16753=CARTESIAN_POINT('Ctrl Pts',(-205.602911672279,-61.638849624479,15.676827380651));
#16754=CARTESIAN_POINT('Ctrl Pts',(-208.15206274551,-63.6863945744461,15.8357356994554));
#16755=CARTESIAN_POINT('Ctrl Pts',(-207.811373989716,-66.9383017123736,
15.9946440182597));
#16756=CARTESIAN_POINT('Ctrl Pts',(-204.893380603372,-68.4130649498665,
16.153552337064));
#16757=CARTESIAN_POINT('Ctrl Pts',(-202.07286371831,-66.7590371605543,16.3124606558683));
#16758=CARTESIAN_POINT('Ctrl Pts',(-201.936470506822,-63.4917903773687,
16.4713689746726));
#16759=CARTESIAN_POINT('Ctrl Pts',(-204.607538235084,-61.608392321744,16.6302772934769));
#16760=CARTESIAN_POINT('Ctrl Pts',(-207.64077536484,-62.8320207279313,16.7891856122812));
#16761=CARTESIAN_POINT('Ctrl Pts',(-208.24805155724,-66.0480436019276,16.9480939310855));
#16762=CARTESIAN_POINT('Ctrl Pts',(-206.674550837501,-67.5419185807874,
17.0540328102884));
#16763=CARTESIAN_POINT('Ctrl Pts',(-205.745932854347,-67.7901775698422,
17.1070022498898));
#16764=CARTESIAN_POINT('Ctrl Pts',(-207.336062657696,-63.0026984430693,
-0.321006749669434));
#16765=CARTESIAN_POINT('Ctrl Pts',(-208.000798179763,-63.7801793522269,
-0.268037310067998));
#16766=CARTESIAN_POINT('Ctrl Pts',(-208.480240995509,-66.0387750109567,
-0.162098430865127));
#16767=CARTESIAN_POINT('Ctrl Pts',(-206.009082789328,-68.4931171380248,
-0.00319011206082034));
#16768=CARTESIAN_POINT('Ctrl Pts',(-202.611389949013,-67.7378152625506,
0.155718206743486));
#16769=CARTESIAN_POINT('Ctrl Pts',(-201.404198517164,-64.4760115003611,
0.314626525547793));
#16770=CARTESIAN_POINT('Ctrl Pts',(-203.493276918295,-61.6929032503864,
0.473534844352099));
#16771=CARTESIAN_POINT('Ctrl Pts',(-206.963857847912,-61.9425259124891,
0.632443163156407));
#16772=CARTESIAN_POINT('Ctrl Pts',(-208.633920228955,-64.9948075983619,
0.791351481960713));
#16773=CARTESIAN_POINT('Ctrl Pts',(-206.972481892344,-68.0520434541846,
0.950259800765019));
#16774=CARTESIAN_POINT('Ctrl Pts',(-203.502676360176,-68.3111058299649,
1.10916811956933));
#16775=CARTESIAN_POINT('Ctrl Pts',(-201.405609072658,-65.5346291225997,
1.26807643837363));
#16776=CARTESIAN_POINT('Ctrl Pts',(-202.603835003667,-62.2679881960402,
1.42698475717794));
#16777=CARTESIAN_POINT('Ctrl Pts',(-205.998840266797,-61.5060359469962,
1.58589307598225));
#16778=CARTESIAN_POINT('Ctrl Pts',(-208.478118943853,-63.9473056488985,
1.74480139478655));
#16779=CARTESIAN_POINT('Ctrl Pts',(-207.768697529891,-67.3536763121769,
1.90370971359086));
#16780=CARTESIAN_POINT('Ctrl Pts',(-204.52096493132,-68.6022216022895,2.06261803239517));
#16781=CARTESIAN_POINT('Ctrl Pts',(-201.712406443479,-66.548290989434,2.22152635119947));
#16782=CARTESIAN_POINT('Ctrl Pts',(-201.917876928207,-63.0749042105964,
2.38043467000378));
#16783=CARTESIAN_POINT('Ctrl Pts',(-204.949003423762,-61.3664238768246,
2.53934298880808));
#16784=CARTESIAN_POINT('Ctrl Pts',(-208.026882997387,-62.9891654522027,
2.69825130761239));
#16785=CARTESIAN_POINT('Ctrl Pts',(-208.329750076191,-66.455417699762,2.8571596264167));
#16786=CARTESIAN_POINT('Ctrl Pts',(-205.579939497992,-68.5873592508376,
3.01606794522101));
#16787=CARTESIAN_POINT('Ctrl Pts',(-202.298446871394,-67.4304499438088,
3.17497626402531));
#16788=CARTESIAN_POINT('Ctrl Pts',(-201.493707957674,-64.0453312890996,
3.33388458282962));
#16789=CARTESIAN_POINT('Ctrl Pts',(-203.90349839961,-61.5354422402711,3.49279290163393));
#16790=CARTESIAN_POINT('Ctrl Pts',(-207.318549253241,-62.2018210220118,
3.65170122043824));
#16791=CARTESIAN_POINT('Ctrl Pts',(-208.607980065528,-65.4335390165435,
3.81060953924254));
#16792=CARTESIAN_POINT('Ctrl Pts',(-206.589655079347,-68.2677932860708,
3.96951785804685));
#16793=CARTESIAN_POINT('Ctrl Pts',(-203.113952083686,-68.1061711944818,
4.12842617685116));
#16794=CARTESIAN_POINT('Ctrl Pts',(-201.367356737724,-65.096846068775,4.28733449565546));
#16795=CARTESIAN_POINT('Ctrl Pts',(-202.951128133319,-61.9987335496681,
4.44624281445977));
#16796=CARTESIAN_POINT('Ctrl Pts',(-206.413282356468,-61.652148567679,4.60515113326408));
#16797=CARTESIAN_POINT('Ctrl Pts',(-208.579755111172,-64.3748363606043,
4.76405945206838));
#16798=CARTESIAN_POINT('Ctrl Pts',(-207.464348390136,-67.6706671908,4.92296777087269));
#16799=CARTESIAN_POINT('Ctrl Pts',(-204.089654608536,-68.5180601899667,
5.08187608967699));
#16800=CARTESIAN_POINT('Ctrl Pts',(-201.549555307088,-66.1401349276025,
5.2407844084813));
#16801=CARTESIAN_POINT('Ctrl Pts',(-202.172785135194,-62.7169467066651,
5.39969272728561));
#16802=CARTESIAN_POINT('Ctrl Pts',(-205.387973952159,-61.3868362278423,
5.55860104608991));
#16803=CARTESIAN_POINT('Ctrl Pts',(-208.247472586089,-63.3692339117493,
5.71750936489423));
#16804=CARTESIAN_POINT('Ctrl Pts',(-208.129724649422,-66.8466997186291,
5.87641768369853));
#16805=CARTESIAN_POINT('Ctrl Pts',(-205.142680134451,-68.6311318636507,
6.03532600250283));
#16806=CARTESIAN_POINT('Ctrl Pts',(-202.024828066921,-67.0865829004874,
6.19423432130715));
#16807=CARTESIAN_POINT('Ctrl Pts',(-201.634580374757,-63.629078055463,6.35314264011145));
#16808=CARTESIAN_POINT('Ctrl Pts',(-204.329711780416,-61.428419126679,6.51205095891576));
#16809=CARTESIAN_POINT('Ctrl Pts',(-207.639355934117,-62.5021456237346,
6.67095927772006));
#16810=CARTESIAN_POINT('Ctrl Pts',(-208.529268066955,-65.8658770949486,
6.82986759652438));
#16811=CARTESIAN_POINT('Ctrl Pts',(-206.183586681908,-68.4357821232429,
6.98877591532867));
#16812=CARTESIAN_POINT('Ctrl Pts',(-202.752806255592,-67.8558005019746,
7.14768423413299));
#16813=CARTESIAN_POINT('Ctrl Pts',(-201.382227937729,-64.6576528991878,
7.30659255293729));
#16814=CARTESIAN_POINT('Ctrl Pts',(-203.328382611466,-61.7733652920829,
7.4655008717416));
#16815=CARTESIAN_POINT('Ctrl Pts',(-206.807057423689,-61.8472203217673,
7.6244091905459));
#16816=CARTESIAN_POINT('Ctrl Pts',(-208.629042186982,-64.811508522489,7.78331750935021));
#16817=CARTESIAN_POINT('Ctrl Pts',(-207.123961634304,-67.9486036030623,
7.94222582815452));
#16818=CARTESIAN_POINT('Ctrl Pts',(-203.671656794376,-68.3824518562811,
8.10113414695882));
#16819=CARTESIAN_POINT('Ctrl Pts',(-201.437162158747,-65.7153060526264,
8.26004246576313));
#16820=CARTESIAN_POINT('Ctrl Pts',(-202.469037434877,-62.3923756547517,
8.41895078456743));
#16821=CARTESIAN_POINT('Ctrl Pts',(-205.821270902666,-61.4600861117225,
8.57785910337174));
#16822=CARTESIAN_POINT('Ctrl Pts',(-208.420572386066,-63.7731500565804,
8.73676742217605));
#16823=CARTESIAN_POINT('Ctrl Pts',(-207.883931336951,-67.2109763173173,
8.89567574098036));
#16824=CARTESIAN_POINT('Ctrl Pts',(-204.703334271224,-68.6218042019629,
9.05458405978466));
#16825=CARTESIAN_POINT('Ctrl Pts',(-201.794717029867,-66.7122024744056,
9.21349237858897));
#16826=CARTESIAN_POINT('Ctrl Pts',(-201.824667390743,-63.2328726552463,
9.37240069739327));
#16827=CARTESIAN_POINT('Ctrl Pts',(-204.76572719775,-61.3736254349403,9.53130901619758));
#16828=CARTESIAN_POINT('Ctrl Pts',(-207.921565691441,-62.8389978846421,
9.69021733500189));
#16829=CARTESIAN_POINT('Ctrl Pts',(-208.398945412955,-66.2855529206304,
9.8491256538062));
#16830=CARTESIAN_POINT('Ctrl Pts',(-205.760209969182,-68.5535274073437,
10.0080339726105));
#16831=CARTESIAN_POINT('Ctrl Pts',(-202.424522522372,-67.5636676840456,
10.1669422914148));
#16832=CARTESIAN_POINT('Ctrl Pts',(-201.450004041473,-64.2234660815981,
10.3258506102191));
#16833=CARTESIAN_POINT('Ctrl Pts',(-203.73008217778,-61.5951820963824,10.4847589290234));
#16834=CARTESIAN_POINT('Ctrl Pts',(-207.17440677989,-62.0883971102576,10.6436672478277));
#16835=CARTESIAN_POINT('Ctrl Pts',(-208.625259549091,-65.2509371110651,
10.802575566632));
#16836=CARTESIAN_POINT('Ctrl Pts',(-206.752514882462,-68.1834207731203,
10.9614838854363));
#16837=CARTESIAN_POINT('Ctrl Pts',(-203.273084159089,-68.1973798508147,
11.1203922042406));
#16838=CARTESIAN_POINT('Ctrl Pts',(-201.376870577281,-65.2800168177356,
11.279300523045));
#16839=CARTESIAN_POINT('Ctrl Pts',(-202.802301555254,-62.1059374958468,
11.4382088418493));
#16840=CARTESIAN_POINT('Ctrl Pts',(-206.242557904149,-61.585102331427,11.5971171606536));
#16841=CARTESIAN_POINT('Ctrl Pts',(-208.543651054332,-64.1950071819504,
11.7560254794579));
#16842=CARTESIAN_POINT('Ctrl Pts',(-207.59596452456,-67.5429204508222,11.9149337982622));
#16843=CARTESIAN_POINT('Ctrl Pts',(-204.268326733228,-68.5595126720785,
12.0738421170665));
#16844=CARTESIAN_POINT('Ctrl Pts',(-201.611478815115,-66.3127834595062,
12.2327504358708));
#16845=CARTESIAN_POINT('Ctrl Pts',(-202.061189246496,-62.8625090439764,
12.3916587546751));
#16846=CARTESIAN_POINT('Ctrl Pts',(-205.205168530226,-61.3718624466171,
12.5505670734794));
#16847=CARTESIAN_POINT('Ctrl Pts',(-208.161051598535,-63.2074518072919,
12.7094753922837));
#16848=CARTESIAN_POINT('Ctrl Pts',(-208.218917891802,-66.6864293160267,
12.868383711088));
#16849=CARTESIAN_POINT('Ctrl Pts',(-205.32571623889,-68.6193072768529,13.0272920298923));
#16850=CARTESIAN_POINT('Ctrl Pts',(-202.133901578945,-67.2340447781946,
13.1862003486966));
#16851=CARTESIAN_POINT('Ctrl Pts',(-201.569693916979,-63.8006349969923,
13.3451086675009));
#16852=CARTESIAN_POINT('Ctrl Pts',(-204.150352533451,-61.4667896441583,
13.5040169863052));
#16853=CARTESIAN_POINT('Ctrl Pts',(-207.509958448151,-62.3721520583455,
13.6629253051096));
#16854=CARTESIAN_POINT('Ctrl Pts',(-208.568462516575,-65.6866960888727,
13.8218336239139));
#16855=CARTESIAN_POINT('Ctrl Pts',(-206.355440022032,-68.371684831825,13.9807419427182));
#16856=CARTESIAN_POINT('Ctrl Pts',(-202.89976528893,-67.9655505816142,14.1396502615225));
#16857=CARTESIAN_POINT('Ctrl Pts',(-201.369562215296,-64.8406327528726,
14.2985585803268));
#16858=CARTESIAN_POINT('Ctrl Pts',(-203.167704028449,-61.8618209334909,
14.4574668991311));
#16859=CARTESIAN_POINT('Ctrl Pts',(-206.64567409827,-61.7600568166538,14.6163752179354));
#16860=CARTESIAN_POINT('Ctrl Pts',(-208.614908982248,-64.6286359675596,
14.7752835367397));
#16861=CARTESIAN_POINT('Ctrl Pts',(-207.270034820723,-67.8376783991727,
14.934191855544));
#16862=CARTESIAN_POINT('Ctrl Pts',(-203.844019947069,-68.4451671656806,
15.0931001743483));
#16863=CARTESIAN_POINT('Ctrl Pts',(-201.477790878185,-65.8941689375223,
15.2520084931526));
#16864=CARTESIAN_POINT('Ctrl Pts',(-202.340691562746,-62.5233988870148,
15.4109168119569));
#16865=CARTESIAN_POINT('Ctrl Pts',(-205.641600447141,-61.4231649792265,
15.5698251307612));
#16866=CARTESIAN_POINT('Ctrl Pts',(-208.354330260832,-63.6021006605898,
15.7287334495655));
#16867=CARTESIAN_POINT('Ctrl Pts',(-207.991779545523,-67.0626823173804,
15.8876417683699));
#16868=CARTESIAN_POINT('Ctrl Pts',(-204.886538848565,-68.6320809475727,
16.0465500871742));
#16869=CARTESIAN_POINT('Ctrl Pts',(-201.885029709121,-66.8719143792362,
16.2054584059785));
#16870=CARTESIAN_POINT('Ctrl Pts',(-201.739884160442,-63.3950087338597,
16.3643667247828));
#16871=CARTESIAN_POINT('Ctrl Pts',(-204.58235400734,-61.3907532347673,16.5232750435871));
#16872=CARTESIAN_POINT('Ctrl Pts',(-207.810233625888,-62.6929017394991,
16.6821833623914));
#16873=CARTESIAN_POINT('Ctrl Pts',(-208.45647866392,-66.1152964431386,16.8410916811957));
#16874=CARTESIAN_POINT('Ctrl Pts',(-206.782006578242,-67.7050332130129,
16.9470305603986));
#16875=CARTESIAN_POINT('Ctrl Pts',(-205.793799282533,-67.9692229537457,
17.));
#16876=CARTESIAN_POINT('Ctrl Pts',(-206.913465996665,-63.364012796625,-1.94289029309402E-15));
#16877=CARTESIAN_POINT('Ctrl Pts',(-206.975064335153,-63.4219001091858,
-1.97292133004108E-15));
#16878=CARTESIAN_POINT('Ctrl Pts',(-207.033290434855,-63.482938938711,-2.21623739315488E-15));
#16879=CARTESIAN_POINT('Ctrl Pts',(-207.088148006259,-63.5467442557774,
-2.20309881449055E-15));
#16880=CARTESIAN_POINT('Ctrl Pts',(-207.14445943011,-63.6122405612339,-2.1896120331214E-15));
#16881=CARTESIAN_POINT('Ctrl Pts',(-207.197221846936,-63.6806523656421,
-1.80211485911159E-15));
#16882=CARTESIAN_POINT('Ctrl Pts',(-207.246413701517,-63.7516117614939,
-1.6306400674182E-15));
#16883=CARTESIAN_POINT('Ctrl Pts',(-207.29736402947,-63.8251077603907,-1.45303552400534E-15));
#16884=CARTESIAN_POINT('Ctrl Pts',(-207.344484547899,-63.9013372602885,
-2.27663609778748E-15));
#16885=CARTESIAN_POINT('Ctrl Pts',(-207.387716218901,-63.9799356548756,
-2.32452945780892E-15));
#16886=CARTESIAN_POINT('Ctrl Pts',(-207.406630074965,-64.0143224525075,
-2.3454828028183E-15));
#16887=CARTESIAN_POINT('Ctrl Pts',(-207.424799084886,-64.0491631801201,
-2.03082216487457E-15));
#16888=CARTESIAN_POINT('Ctrl Pts',(-207.442215847947,-64.084429403981,-2.04697370165263E-15));
#16889=CARTESIAN_POINT('Ctrl Pts',(-207.4516722521,-64.1035771448449,-2.05574315318221E-15));
#16890=CARTESIAN_POINT('Ctrl Pts',(-207.460906871958,-64.1228503386334,
-2.04057437215808E-15));
#16891=CARTESIAN_POINT('Ctrl Pts',(-207.469918322462,-64.1422445609559,
-2.04697370165263E-15));
#16892=CARTESIAN_POINT('Ctrl Pts',(-207.478568225495,-64.1608606696942,
-2.05311628431163E-15));
#16893=CARTESIAN_POINT('Ctrl Pts',(-207.487014999459,-64.1795942961117,
-2.37355651913976E-15));
#16894=CARTESIAN_POINT('Ctrl Pts',(-207.495243316265,-64.1984087222124,
-2.34534613952064E-15));
#16895=CARTESIAN_POINT('Ctrl Pts',(-207.531786155502,-64.281965610518,-2.22006081185391E-15));
#16896=CARTESIAN_POINT('Ctrl Pts',(-207.564069529394,-64.3672061702463,
-2.19854429085911E-15));
#16897=CARTESIAN_POINT('Ctrl Pts',(-207.592069829017,-64.4537311766029,
-2.15105711021124E-15));
#16898=CARTESIAN_POINT('Ctrl Pts',(-207.620534398179,-64.5416908434951,
-2.10278255043571E-15));
#16899=CARTESIAN_POINT('Ctrl Pts',(-207.644573172372,-64.6309786604899,
-2.09454222238891E-15));
#16900=CARTESIAN_POINT('Ctrl Pts',(-207.664122231294,-64.7212123541091,
-2.12330153459561E-15));
#16901=CARTESIAN_POINT('Ctrl Pts',(-207.68337365362,-64.8100722297138,-2.15162298307744E-15));
#16902=CARTESIAN_POINT('Ctrl Pts',(-207.698271307414,-64.8998503076178,
-2.67974986921836E-15));
#16903=CARTESIAN_POINT('Ctrl Pts',(-207.708711137774,-64.9902045182676,
-2.76167977375508E-15));
#16904=CARTESIAN_POINT('Ctrl Pts',(-207.712805437947,-65.0256396975281,
-2.79381110259042E-15));
#16905=CARTESIAN_POINT('Ctrl Pts',(-207.716213605543,-65.0611636688123,
-2.0404376105344E-15));
#16906=CARTESIAN_POINT('Ctrl Pts',(-207.718927373463,-65.0967563226444,
-2.02615701994091E-15));
#16907=CARTESIAN_POINT('Ctrl Pts',(-207.720523200181,-65.1176865236056,
-2.01775934236463E-15));
#16908=CARTESIAN_POINT('Ctrl Pts',(-207.721878881011,-65.1386404789908,
-1.74090680682343E-15));
#16909=CARTESIAN_POINT('Ctrl Pts',(-207.72299254181,-65.1596141213673,-1.72084568816899E-15));
#16910=CARTESIAN_POINT('Ctrl Pts',(-207.723754218348,-65.1739588224918,
-1.70712509800373E-15));
#16911=CARTESIAN_POINT('Ctrl Pts',(-207.724402620351,-65.1883131146187,
-1.95724670614016E-15));
#16912=CARTESIAN_POINT('Ctrl Pts',(-207.724936762549,-65.2026603377787,
-1.95676808090184E-15));
#16913=CARTESIAN_POINT('Ctrl Pts',(-207.728480618606,-65.2978493977624,
-1.95359256142936E-15));
#16914=CARTESIAN_POINT('Ctrl Pts',(-207.727008196039,-65.3928884344764,
-1.81199077416004E-15));
#16915=CARTESIAN_POINT('Ctrl Pts',(-207.720461583985,-65.4873781558944,
-1.85962356624714E-15));
#16916=CARTESIAN_POINT('Ctrl Pts',(-207.713936993971,-65.5815500248844,
-1.9070961271642E-15));
#16917=CARTESIAN_POINT('Ctrl Pts',(-207.702372653513,-65.6751772225213,
-2.05958830061839E-15));
#16918=CARTESIAN_POINT('Ctrl Pts',(-207.685663242701,-65.767882393997,-1.99840144432528E-15));
#16919=CARTESIAN_POINT('Ctrl Pts',(-207.683580478217,-65.7794377409136,
-1.99077473548103E-15));
#16920=CARTESIAN_POINT('Ctrl Pts',(-207.681417710998,-65.7909787747085,
-2.33792174055657E-15));
#16921=CARTESIAN_POINT('Ctrl Pts',(-207.679174680234,-65.8025047726911,
-2.35922392732846E-15));
#16922=CARTESIAN_POINT('Ctrl Pts',(-207.661554445533,-65.8930477972969,
-2.52759723237176E-15));
#16923=CARTESIAN_POINT('Ctrl Pts',(-207.638985550185,-65.9826632848584,
-1.79135627445481E-15));
#16924=CARTESIAN_POINT('Ctrl Pts',(-207.611743048214,-66.0711138579085,
-1.66533453693773E-15));
#16925=CARTESIAN_POINT('Ctrl Pts',(-207.60081644828,-66.1065901892194,-1.61478891853904E-15));
#16926=CARTESIAN_POINT('Ctrl Pts',(-207.589137410261,-66.1418790674857,
-1.79168624825887E-15));
#16927=CARTESIAN_POINT('Ctrl Pts',(-207.576721387245,-66.1769648121992,
-1.77635683940025E-15));
#16928=CARTESIAN_POINT('Ctrl Pts',(-207.570942246212,-66.1932957634797,
-1.76922163872903E-15));
#16929=CARTESIAN_POINT('Ctrl Pts',(-207.565003418531,-66.2095827012965,
-1.91957011249023E-15));
#16930=CARTESIAN_POINT('Ctrl Pts',(-207.558906371455,-66.2258240187521,
-1.9151347174784E-15));
#16931=CARTESIAN_POINT('Ctrl Pts',(-207.553840425172,-66.2393186893321,
-1.91144941333107E-15));
#16932=CARTESIAN_POINT('Ctrl Pts',(-207.548668567227,-66.2527729916654,
-2.42723306653759E-15));
#16933=CARTESIAN_POINT('Ctrl Pts',(-207.543392857624,-66.2661841275907,
-2.41473507855972E-15));
#16934=CARTESIAN_POINT('Ctrl Pts',(-207.509159374317,-66.3532074727684,
-2.33363704720111E-15));
#16935=CARTESIAN_POINT('Ctrl Pts',(-207.470547395912,-66.4384398905487,
-2.12854475574276E-15));
#16936=CARTESIAN_POINT('Ctrl Pts',(-207.427889442439,-66.5216501935512,
-2.16493489801906E-15));
#16937=CARTESIAN_POINT('Ctrl Pts',(-207.38365247829,-66.6079405776665,-2.20267204404216E-15));
#16938=CARTESIAN_POINT('Ctrl Pts',(-207.335064336909,-66.692057101939,-2.12399586674231E-15));
#16939=CARTESIAN_POINT('Ctrl Pts',(-207.282439886309,-66.773738360666,-2.05391259555654E-15));
#16940=CARTESIAN_POINT('Ctrl Pts',(-207.229239181682,-66.8563140544646,
-1.98306189085347E-15));
#16941=CARTESIAN_POINT('Ctrl Pts',(-207.171912867569,-66.9364016733955,
-1.93693493431011E-15));
#16942=CARTESIAN_POINT('Ctrl Pts',(-207.110734661138,-67.0137157330808,
-1.9151347174784E-15));
#16943=CARTESIAN_POINT('Ctrl Pts',(-207.086644405525,-67.0441598335049,
-1.90655040573494E-15));
#16944=CARTESIAN_POINT('Ctrl Pts',(-207.061956365489,-67.0741736421049,
-2.23389407293862E-15));
#16945=CARTESIAN_POINT('Ctrl Pts',(-207.036685317581,-67.1037386472167,
-2.27595720048157E-15));
#16946=CARTESIAN_POINT('Ctrl Pts',(-207.022376522802,-67.1204787362049,
-2.29977388833693E-15));
#16947=CARTESIAN_POINT('Ctrl Pts',(-207.007880798569,-67.1370749273764,
-2.22822292691737E-15));
#16948=CARTESIAN_POINT('Ctrl Pts',(-206.993200685982,-67.1535237511539,
-2.22044604925031E-15));
#16949=CARTESIAN_POINT('Ctrl Pts',(-206.979145852523,-67.1692719599935,
-2.21300041694992E-15));
#16950=CARTESIAN_POINT('Ctrl Pts',(-206.964919138242,-67.1848880123012,
-1.95342784401499E-15));
#16951=CARTESIAN_POINT('Ctrl Pts',(-206.950541882912,-67.2003486168303,
-1.97064586870965E-15));
#16952=CARTESIAN_POINT('Ctrl Pts',(-206.881822930974,-67.2742456517767,
-2.05294284294357E-15));
#16953=CARTESIAN_POINT('Ctrl Pts',(-206.809592725806,-67.3446809429097,
-2.39171272535874E-15));
#16954=CARTESIAN_POINT('Ctrl Pts',(-206.734164841959,-67.4113677334851,
-2.22044604925031E-15));
#16955=CARTESIAN_POINT('Ctrl Pts',(-206.66904943858,-67.4689371235679,-2.07259490811688E-15));
#16956=CARTESIAN_POINT('Ctrl Pts',(-206.6015499159,-67.5237130159225,-1.84853531005696E-15));
#16957=CARTESIAN_POINT('Ctrl Pts',(-206.531841458199,-67.5754953714549,
-1.72084568816899E-15));
#16958=CARTESIAN_POINT('Ctrl Pts',(-206.504681281771,-67.595671085543,-1.67109458517742E-15));
#16959=CARTESIAN_POINT('Ctrl Pts',(-206.477185531439,-67.6153921679212,
-1.55730478202358E-15));
#16960=CARTESIAN_POINT('Ctrl Pts',(-206.449363702133,-67.6346459831098,
-1.55431223447522E-15));
#16961=CARTESIAN_POINT('Ctrl Pts',(-206.43409331051,-67.6452137029715,-1.55266973381473E-15));
#16962=CARTESIAN_POINT('Ctrl Pts',(-206.418725944916,-67.6556396822825,
-1.84911424756666E-15));
#16963=CARTESIAN_POINT('Ctrl Pts',(-206.403273354045,-67.6659153349133,
-1.83186799063151E-15));
#16964=CARTESIAN_POINT('Ctrl Pts',(-206.316688603458,-67.7234923993424,
-1.73523287825519E-15));
#16965=CARTESIAN_POINT('Ctrl Pts',(-206.227347132085,-67.7764114036352,
-1.8361507155124E-15));
#16966=CARTESIAN_POINT('Ctrl Pts',(-206.135558921451,-67.8243493290082,
-1.33226762955019E-15));
#16967=CARTESIAN_POINT('Ctrl Pts',(-206.043770710818,-67.8722872543811,
-8.28384543587972E-16));
#16968=CARTESIAN_POINT('Ctrl Pts',(-205.949535108699,-67.915245019694,-3.68147691493984E-16));
#16969=CARTESIAN_POINT('Ctrl Pts',(-205.853123870327,-67.9528583595717,
-2.22044604925031E-16));
#16970=CARTESIAN_POINT('Ctrl Pts',(-205.834023285542,-67.9603101546064,
-1.93099282372341E-16));
#16971=CARTESIAN_POINT('Ctrl Pts',(-205.814837205121,-67.9675520267903,
-1.66533453693773E-16));
#16972=CARTESIAN_POINT('Ctrl Pts',(-205.795568749511,-67.9745849194645,
-1.66533453693773E-16));
#16973=CARTESIAN_POINT('Ctrl Pts',(-202.480291602729,-65.0019224916823,
1.61258330249198));
#16974=CARTESIAN_POINT('Ctrl Pts',(-202.47924620393,-65.1255297484548,1.60474993100901));
#16975=CARTESIAN_POINT('Ctrl Pts',(-202.487554213272,-65.248995872321,1.59691655952604));
#16976=CARTESIAN_POINT('Ctrl Pts',(-202.505700651816,-65.3709985616315,
1.58908318804307));
#16977=CARTESIAN_POINT('Ctrl Pts',(-202.628407290015,-66.1959835756441,
1.53611374844163));
#16978=CARTESIAN_POINT('Ctrl Pts',(-203.200975686124,-66.9540531066665,
1.48314430884019));
#16979=CARTESIAN_POINT('Ctrl Pts',(-203.960945445007,-67.2977215942629,
1.43017486923876));
#16980=CARTESIAN_POINT('Ctrl Pts',(-204.72091520389,-67.6413900818592,1.37720542963732));
#16981=CARTESIAN_POINT('Ctrl Pts',(-205.668286325546,-67.5706575260295,
1.32423599003589));
#16982=CARTESIAN_POINT('Ctrl Pts',(-206.368785563095,-67.1179282381352,
1.27126655043445));
#16983=CARTESIAN_POINT('Ctrl Pts',(-207.069284800645,-66.6651989502408,
1.21829711083302));
#16984=CARTESIAN_POINT('Ctrl Pts',(-207.522912154087,-65.8304729302817,
1.16532767123158));
#16985=CARTESIAN_POINT('Ctrl Pts',(-207.521734830089,-64.9964232360559,
1.11235823163015));
#16986=CARTESIAN_POINT('Ctrl Pts',(-207.52055750609,-64.1623735418301,1.05938879202871));
#16987=CARTESIAN_POINT('Ctrl Pts',(-207.064575504651,-63.3290001733376,
1.00641935242727));
#16988=CARTESIAN_POINT('Ctrl Pts',(-206.362793088589,-62.8782358874513,
0.953449912825839));
#16989=CARTESIAN_POINT('Ctrl Pts',(-205.661010672528,-62.427471601565,0.900480473224403));
#16990=CARTESIAN_POINT('Ctrl Pts',(-204.713427841845,-62.359316398285,0.847511033622967));
#16991=CARTESIAN_POINT('Ctrl Pts',(-203.954442842921,-62.7051788768636,
0.794541594021531));
#16992=CARTESIAN_POINT('Ctrl Pts',(-203.195457843997,-63.0510413554422,
0.741572154420096));
#16993=CARTESIAN_POINT('Ctrl Pts',(-202.625070676832,-63.8109215158794,
0.68860271481866));
#16994=CARTESIAN_POINT('Ctrl Pts',(-202.504678591524,-64.6361514920533,
0.635633275217225));
#16995=CARTESIAN_POINT('Ctrl Pts',(-202.487215476291,-64.7558527675182,
0.627949950975476));
#16996=CARTESIAN_POINT('Ctrl Pts',(-202.47922029748,-64.8769290089006,0.620266626733727));
#16997=CARTESIAN_POINT('Ctrl Pts',(-202.480232352617,-64.9981364767374,
0.612583302491977));
#16998=CARTESIAN_POINT('Ctrl Pts',(-204.206200717467,-67.9692229537457,
-8.32667268468867E-16));
#16999=CARTESIAN_POINT('Ctrl Pts',(-203.217993421758,-67.705033213013,0.0529694396014348));
#17000=CARTESIAN_POINT('Ctrl Pts',(-201.543521285756,-66.115296794048,0.158908318804306));
#17001=CARTESIAN_POINT('Ctrl Pts',(-202.189766417583,-62.6929016513152,
0.317816637608613));
#17002=CARTESIAN_POINT('Ctrl Pts',(-205.417645988708,-61.3907533400893,
0.47672495641292));
#17003=CARTESIAN_POINT('Ctrl Pts',(-208.260115801475,-63.3950087136501,
0.635633275217226));
#17004=CARTESIAN_POINT('Ctrl Pts',(-208.114970263096,-66.8719143799143,
0.794541594021533));
#17005=CARTESIAN_POINT('Ctrl Pts',(-205.113461147179,-68.6320808995075,
0.95344991282584));
#17006=CARTESIAN_POINT('Ctrl Pts',(-202.008220487258,-67.0626823018313,
1.11235823163015));
#17007=CARTESIAN_POINT('Ctrl Pts',(-201.645669772482,-63.602100671981,1.27126655043445));
#17008=CARTESIAN_POINT('Ctrl Pts',(-204.358399560164,-61.4231650176065,
1.43017486923876));
#17009=CARTESIAN_POINT('Ctrl Pts',(-207.659308409489,-62.5233989116837,
1.58908318804307));
#17010=CARTESIAN_POINT('Ctrl Pts',(-208.522209085787,-65.8941689287448,
1.74799150684737));
#17011=CARTESIAN_POINT('Ctrl Pts',(-206.155980040914,-68.445167130006,1.90689982565168));
#17012=CARTESIAN_POINT('Ctrl Pts',(-202.729965202703,-67.8376783700826,
2.06580814445599));
#17013=CARTESIAN_POINT('Ctrl Pts',(-201.385091054919,-64.6286359713235,
2.22471646326029));
#17014=CARTESIAN_POINT('Ctrl Pts',(-203.354325918685,-61.7600568500266,
2.3836247820646));
#17015=CARTESIAN_POINT('Ctrl Pts',(-206.832295952684,-61.8618209657714,
2.54253310086891));
#17016=CARTESIAN_POINT('Ctrl Pts',(-208.630437747347,-64.8406327545204,
2.70144141967322));
#17017=CARTESIAN_POINT('Ctrl Pts',(-207.100234689454,-67.965550551091,2.86034973847752));
#17018=CARTESIAN_POINT('Ctrl Pts',(-203.644559991919,-68.3716847971282,
3.01925805728183));
#17019=CARTESIAN_POINT('Ctrl Pts',(-201.431537520148,-65.6866960818049,
3.17816637608613));
#17020=CARTESIAN_POINT('Ctrl Pts',(-202.49004157768,-62.3721520853899,3.33707469489044));
#17021=CARTESIAN_POINT('Ctrl Pts',(-205.849647457805,-61.4667896805192,
3.49598301369474));
#17022=CARTESIAN_POINT('Ctrl Pts',(-208.430306047719,-63.8006350093353,
3.65489133249905));
#17023=CARTESIAN_POINT('Ctrl Pts',(-207.86609839156,-67.2340447552034,3.81379965130336));
#17024=CARTESIAN_POINT('Ctrl Pts',(-204.674283764462,-68.6193072396057,
3.97270797010767));
#17025=CARTESIAN_POINT('Ctrl Pts',(-201.781082141325,-66.6864292986713,
4.13161628891197));
#17026=CARTESIAN_POINT('Ctrl Pts',(-201.838948433996,-63.2074518257396,
4.29052460771628));
#17027=CARTESIAN_POINT('Ctrl Pts',(-204.794831471885,-61.3718624839552,
4.44943292652058));
#17028=CARTESIAN_POINT('Ctrl Pts',(-207.93881072326,-62.8625090659739,4.6083412453249));
#17029=CARTESIAN_POINT('Ctrl Pts',(-208.388521150012,-66.3127834459959,
4.7672495641292));
#17030=CARTESIAN_POINT('Ctrl Pts',(-205.731673259242,-68.5595126354467,
4.92615788293351));
#17031=CARTESIAN_POINT('Ctrl Pts',(-202.404035502155,-67.5429204246525,
5.08506620173781));
#17032=CARTESIAN_POINT('Ctrl Pts',(-201.456348982136,-64.1950071902349,
5.24397452054212));
#17033=CARTESIAN_POINT('Ctrl Pts',(-203.757442108639,-61.5851023665706,
5.40288283934643));
#17034=CARTESIAN_POINT('Ctrl Pts',(-207.197698422129,-62.1059375256302,
5.56179115815073));
#17035=CARTESIAN_POINT('Ctrl Pts',(-208.623129385432,-65.2800168148538,
5.72069947695504));
#17036=CARTESIAN_POINT('Ctrl Pts',(-206.726915823139,-68.1973798179096,
5.87960779575935));
#17037=CARTESIAN_POINT('Ctrl Pts',(-203.247485135573,-68.183420740359,6.03851611456365));
#17038=CARTESIAN_POINT('Ctrl Pts',(-201.374740488217,-65.2509371084826,
6.19742443336796));
#17039=CARTESIAN_POINT('Ctrl Pts',(-202.825593242488,-62.0883971402218,
6.35633275217227));
#17040=CARTESIAN_POINT('Ctrl Pts',(-206.26991780915,-61.5951821314221,6.51524107097657));
#17041=CARTESIAN_POINT('Ctrl Pts',(-208.549995921993,-64.2234660895895,
6.67414938978088));
#17042=CARTESIAN_POINT('Ctrl Pts',(-207.575477451123,-67.5636676576622,
6.83305770858519));
#17043=CARTESIAN_POINT('Ctrl Pts',(-204.239790038642,-68.5535273707736,
6.9919660273895));
#17044=CARTESIAN_POINT('Ctrl Pts',(-201.601054622025,-66.2855529074004,
7.15087434619379));
#17045=CARTESIAN_POINT('Ctrl Pts',(-202.078434338626,-62.8389979068817,
7.30978266499812));
#17046=CARTESIAN_POINT('Ctrl Pts',(-205.234272799839,-61.3736254722602,
7.46869098380241));
#17047=CARTESIAN_POINT('Ctrl Pts',(-208.175332576579,-63.2328726734323,
7.62759930260673));
#17048=CARTESIAN_POINT('Ctrl Pts',(-208.205282937147,-66.7122024567848,
7.78650762141103));
#17049=CARTESIAN_POINT('Ctrl Pts',(-205.296665725724,-68.62180416469,7.94541594021533));
#17050=CARTESIAN_POINT('Ctrl Pts',(-202.116068692728,-67.2109762945637,
8.10432425901964));
#17051=CARTESIAN_POINT('Ctrl Pts',(-201.579427649136,-63.7731500692063,
8.26323257782395));
#17052=CARTESIAN_POINT('Ctrl Pts',(-204.178729105786,-61.4600861481526,
8.42214089662826));
#17053=CARTESIAN_POINT('Ctrl Pts',(-207.530962539076,-62.3923756815873,
8.58104921543256));
#17054=CARTESIAN_POINT('Ctrl Pts',(-208.562837804587,-65.7153060452649,
8.73995753423686));
#17055=CARTESIAN_POINT('Ctrl Pts',(-206.328343191953,-68.3824518214713,
8.89886585304117));
#17056=CARTESIAN_POINT('Ctrl Pts',(-202.876038387555,-67.9486035727176,
9.05777417184548));
#17057=CARTESIAN_POINT('Ctrl Pts',(-201.370957850366,-64.8115085244288,
9.21668249064979));
#17058=CARTESIAN_POINT('Ctrl Pts',(-203.192942594908,-61.8472203542135,
9.3755908094541));
#17059=CARTESIAN_POINT('Ctrl Pts',(-206.671617371331,-61.7733653252889,
9.5344991282584));
#17060=CARTESIAN_POINT('Ctrl Pts',(-208.61777202504,-64.6576529027109,9.69340744706271));
#17061=CARTESIAN_POINT('Ctrl Pts',(-207.247193721282,-67.8558004725847,
9.85231576586701));
#17062=CARTESIAN_POINT('Ctrl Pts',(-203.816413330272,-68.4357820878843,
10.0112240846713));
#17063=CARTESIAN_POINT('Ctrl Pts',(-201.470731969365,-65.8658770860377,
10.1701324034756));
#17064=CARTESIAN_POINT('Ctrl Pts',(-202.360644093045,-62.5021456494408,
10.3290407222799));
#17065=CARTESIAN_POINT('Ctrl Pts',(-205.670288212686,-61.4284191634349,
10.4879490410842));
#17066=CARTESIAN_POINT('Ctrl Pts',(-208.365419590609,-63.6290780695714,
10.6468573598886));
#17067=CARTESIAN_POINT('Ctrl Pts',(-207.975171902461,-67.0865828790137,
10.8057656786928));
#17068=CARTESIAN_POINT('Ctrl Pts',(-204.857319867018,-68.6311318262819,
10.9646739974972));
#17069=CARTESIAN_POINT('Ctrl Pts',(-201.870275382787,-66.8466996996243,
11.1235823163015));
#17070=CARTESIAN_POINT('Ctrl Pts',(-201.752527447332,-63.3692339285321,
11.2824906351058));
#17071=CARTESIAN_POINT('Ctrl Pts',(-204.612026051834,-61.3868362650263,
11.4413989539101));
#17072=CARTESIAN_POINT('Ctrl Pts',(-207.82721483571,-62.7169467301605,11.6003072727144));
#17073=CARTESIAN_POINT('Ctrl Pts',(-208.450444657403,-66.140134915869,11.7592155915187));
#17074=CARTESIAN_POINT('Ctrl Pts',(-205.910345382095,-68.5180601537614,
11.918123910323));
#17075=CARTESIAN_POINT('Ctrl Pts',(-202.535651635225,-67.6706671633156,
12.0770322291273));
#17076=CARTESIAN_POINT('Ctrl Pts',(-201.420244925668,-64.3748363670382,
12.2359405479316));
#17077=CARTESIAN_POINT('Ctrl Pts',(-203.586717658077,-61.6521486021326,
12.3948488667359));
#17078=CARTESIAN_POINT('Ctrl Pts',(-207.048871845595,-61.9987335805548,
12.5537571855402));
#17079=CARTESIAN_POINT('Ctrl Pts',(-208.632643224891,-65.0968460677781,
12.7126655043445));
#17080=CARTESIAN_POINT('Ctrl Pts',(-206.886047896905,-68.1061711625154,
12.8715738231488));
#17081=CARTESIAN_POINT('Ctrl Pts',(-203.410344937013,-68.2677932524411,
13.0304821419532));
#17082=CARTESIAN_POINT('Ctrl Pts',(-201.392019971602,-65.433539012082,13.1893904607574));
#17083=CARTESIAN_POINT('Ctrl Pts',(-202.68145077062,-62.2018210508086,13.3482987795618));
#17084=CARTESIAN_POINT('Ctrl Pts',(-206.096501589105,-61.5354422759257,
13.5072070983661));
#17085=CARTESIAN_POINT('Ctrl Pts',(-208.506292006242,-64.0453312989241,
13.6661154171704));
#17086=CARTESIAN_POINT('Ctrl Pts',(-207.701553100804,-67.4304499187966,
13.8250237359747));
#17087=CARTESIAN_POINT('Ctrl Pts',(-204.420060507976,-68.5873592139186,
13.983932054779));
#17088=CARTESIAN_POINT('Ctrl Pts',(-201.670249958077,-66.4554176847852,
14.1428403735833));
#17089=CARTESIAN_POINT('Ctrl Pts',(-201.973117033763,-62.9891654728944,
14.3017486923876));
#17090=CARTESIAN_POINT('Ctrl Pts',(-205.050996575713,-61.3664239142234,
14.4606570111919));
#17091=CARTESIAN_POINT('Ctrl Pts',(-208.082123040074,-63.0749042303987,
14.6195653299962));
#17092=CARTESIAN_POINT('Ctrl Pts',(-208.287593522688,-66.548290973518,14.7784736488005));
#17093=CARTESIAN_POINT('Ctrl Pts',(-205.479035063749,-68.6022215651833,
14.9373819676048));
#17094=CARTESIAN_POINT('Ctrl Pts',(-202.231302498607,-67.3536762880221,
15.0962902864091));
#17095=CARTESIAN_POINT('Ctrl Pts',(-201.521881091931,-63.9473056596023,
15.2551986052134));
#17096=CARTESIAN_POINT('Ctrl Pts',(-204.001159743508,-61.5060359832025,
15.4141069240177));
#17097=CARTESIAN_POINT('Ctrl Pts',(-207.396164971614,-62.2679882236812,
15.5730152428221));
#17098=CARTESIAN_POINT('Ctrl Pts',(-208.594390890487,-65.5346291179969,
15.7319235616264));
#17099=CARTESIAN_POINT('Ctrl Pts',(-206.497323624104,-68.3111057941983,
15.8908318804307));
#17100=CARTESIAN_POINT('Ctrl Pts',(-203.027518128658,-68.0520434259267,
16.049740199235));
#17101=CARTESIAN_POINT('Ctrl Pts',(-201.366079806868,-64.9948075926078,
16.2086485180393));
#17102=CARTESIAN_POINT('Ctrl Pts',(-203.036142175806,-61.9425259545107,
16.3675568368436));
#17103=CARTESIAN_POINT('Ctrl Pts',(-206.506723058425,-61.6929032655643,
16.5264651556479));
#17104=CARTESIAN_POINT('Ctrl Pts',(-208.5958014629,-64.4760115385876,16.6853734744522));
#17105=CARTESIAN_POINT('Ctrl Pts',(-207.388609988071,-67.7378151779928,
16.8442817932565));
#17106=CARTESIAN_POINT('Ctrl Pts',(-203.990917296448,-68.4931171860738,
17.0031901120608));
#17107=CARTESIAN_POINT('Ctrl Pts',(-201.519758764249,-66.038774750277,17.1620984308651));
#17108=CARTESIAN_POINT('Ctrl Pts',(-201.999201820237,-63.780179352227,17.268037310068));
#17109=CARTESIAN_POINT('Ctrl Pts',(-202.663937342304,-63.0026984430694,
17.3210067496694));
#17110=CARTESIAN_POINT('Ctrl Pts',(-204.254067145653,-67.7901775698422,
-0.107002249889811));
#17111=CARTESIAN_POINT('Ctrl Pts',(-203.325449162499,-67.5419185807875,
-0.0540328102883759));
#17112=CARTESIAN_POINT('Ctrl Pts',(-201.751948395471,-66.0480439316771,
0.0519060689144955));
#17113=CARTESIAN_POINT('Ctrl Pts',(-202.359224676009,-62.8320206450648,
0.210814387718802));
#17114=CARTESIAN_POINT('Ctrl Pts',(-205.392461761202,-61.6083924207151,
0.369722706523109));
#17115=CARTESIAN_POINT('Ctrl Pts',(-208.063529457392,-63.4917903583777,
0.528631025327416));
#17116=CARTESIAN_POINT('Ctrl Pts',(-207.927136255583,-66.7590371611916,
0.687539344131722));
#17117=CARTESIAN_POINT('Ctrl Pts',(-205.106619392628,-68.4130649046996,
0.846447662936029));
#17118=CARTESIAN_POINT('Ctrl Pts',(-202.188626041087,-66.9383016977623,
1.00535598174034));
#17119=CARTESIAN_POINT('Ctrl Pts',(-201.847937285795,-63.6863945851504,
1.16426430054464));
#17120=CARTESIAN_POINT('Ctrl Pts',(-204.397088334585,-61.6388496605446,
1.32317261934895));
#17121=CARTESIAN_POINT('Ctrl Pts',(-207.498951002008,-62.6727389914087,
1.48208093815326));
#17122=CARTESIAN_POINT('Ctrl Pts',(-208.309818407223,-65.8402501689831,
1.64098925695756));
#17123=CARTESIAN_POINT('Ctrl Pts',(-206.08627396177,-68.2374221135446,1.79989757576187));
#17124=CARTESIAN_POINT('Ctrl Pts',(-202.866849248828,-67.6665651795,1.95880589456618));
#17125=CARTESIAN_POINT('Ctrl Pts',(-201.603071573705,-64.651029377315,2.11771421337048));
#17126=CARTESIAN_POINT('Ctrl Pts',(-203.453560752936,-61.9554267748013,
2.27662253217479));
#17127=CARTESIAN_POINT('Ctrl Pts',(-206.721807741666,-62.0510544718753,
2.43553085097909));
#17128=CARTESIAN_POINT('Ctrl Pts',(-208.4115208353,-64.8502426659663,2.59443916978341));
#17129=CARTESIAN_POINT('Ctrl Pts',(-206.973589660732,-67.7867266146009,
2.75334748858771));
#17130=CARTESIAN_POINT('Ctrl Pts',(-203.726293590367,-68.1683707960215,
2.91225580739202));
#17131=CARTESIAN_POINT('Ctrl Pts',(-201.646717297687,-65.6452880213436,
3.07116412619632));
#17132=CARTESIAN_POINT('Ctrl Pts',(-202.641393118574,-62.5306124118932,
3.23007244500063));
#17133=CARTESIAN_POINT('Ctrl Pts',(-205.798413361331,-61.6798437380682,
3.38898076380494));
#17134=CARTESIAN_POINT('Ctrl Pts',(-208.223457160724,-63.8729572190647,
3.54788908260924));
#17135=CARTESIAN_POINT('Ctrl Pts',(-207.693271461815,-67.0993309236441,
3.70679740141355));
#17136=CARTESIAN_POINT('Ctrl Pts',(-204.693924589467,-68.4010615018235,
3.86570572021786));
#17137=CARTESIAN_POINT('Ctrl Pts',(-201.975184232255,-66.5847369077965,
4.02461403902216));
#17138=CARTESIAN_POINT('Ctrl Pts',(-202.029561163317,-63.3155432291222,
4.18352235782647));
#17139=CARTESIAN_POINT('Ctrl Pts',(-204.807203219798,-61.5906406910937,
4.34243067663077));
#17140=CARTESIAN_POINT('Ctrl Pts',(-207.761599209553,-62.9914006618004,
4.50133899543508));
#17141=CARTESIAN_POINT('Ctrl Pts',(-208.184191909797,-66.2336220560524,
4.66024731423939));
#17142=CARTESIAN_POINT('Ctrl Pts',(-205.687553056201,-68.3448725372624,
4.8191556330437));
#17143=CARTESIAN_POINT('Ctrl Pts',(-202.560573245315,-67.3895812612549,
4.978063951848));
#17144=CARTESIAN_POINT('Ctrl Pts',(-201.670032618157,-64.2435485927867,
5.13697227065231));
#17145=CARTESIAN_POINT('Ctrl Pts',(-203.832368868315,-61.7910221197497,
5.29588058945662));
#17146=CARTESIAN_POINT('Ctrl Pts',(-207.06517628963,-62.2804507012443,5.45478890826092));
#17147=CARTESIAN_POINT('Ctrl Pts',(-208.404653170661,-65.2631316839978,
5.61369722706523));
#17148=CARTESIAN_POINT('Ctrl Pts',(-206.622782077934,-68.0045764798305,
5.77260554586953));
#17149=CARTESIAN_POINT('Ctrl Pts',(-203.353162513657,-67.9914591404848,
5.93151386467385));
#17150=CARTESIAN_POINT('Ctrl Pts',(-201.593345150497,-65.235805496063,6.09042218347814));
#17151=CARTESIAN_POINT('Ctrl Pts',(-202.956710877885,-62.2639680083999,
6.24933050228247));
#17152=CARTESIAN_POINT('Ctrl Pts',(-206.193341235007,-61.8004940705718,
6.40823882108676));
#17153=CARTESIAN_POINT('Ctrl Pts',(-208.335929685604,-64.2702914086274,
6.56714713989107));
#17154=CARTESIAN_POINT('Ctrl Pts',(-207.420175085435,-67.4090774274512,
6.72605545869537));
#17155=CARTESIAN_POINT('Ctrl Pts',(-204.285631016736,-68.3392481865482,
6.88496377749969));
#17156=CARTESIAN_POINT('Ctrl Pts',(-201.806012447539,-66.2080335303043,
7.04387209630399));
#17157=CARTESIAN_POINT('Ctrl Pts',(-202.2546059679,-62.9693072354186,7.20278041510831));
#17158=CARTESIAN_POINT('Ctrl Pts',(-205.220146052188,-61.5922973704678,
7.3616887339126));
#17159=CARTESIAN_POINT('Ctrl Pts',(-207.983858696358,-63.3394311890845,
7.52059705271692));
#17160=CARTESIAN_POINT('Ctrl Pts',(-208.012003037678,-66.6089559337142,
7.67950537152122));
#17161=CARTESIAN_POINT('Ctrl Pts',(-205.27877665859,-68.4034078612826,7.83841369032552));
#17162=CARTESIAN_POINT('Ctrl Pts',(-202.289970954736,-67.0776535008131,
7.99732200912983));
#17163=CARTESIAN_POINT('Ctrl Pts',(-201.785689590146,-63.8471296323018,
8.15623032793414));
#17164=CARTESIAN_POINT('Ctrl Pts',(-204.228252083627,-61.6735444315025,
8.31513864673845));
#17165=CARTESIAN_POINT('Ctrl Pts',(-207.378344441172,-62.5496165167955,
8.47404696554275));
#17166=CARTESIAN_POINT('Ctrl Pts',(-208.347997197315,-65.6721727920609,
8.63295528434706));
#17167=CARTESIAN_POINT('Ctrl Pts',(-206.248243542832,-68.1784885643011,
8.79186360315136));
#17168=CARTESIAN_POINT('Ctrl Pts',(-203.00411415964,-67.7708015460996,8.95077192195566));
#17169=CARTESIAN_POINT('Ctrl Pts',(-201.589790607288,-64.82287463911,9.10968024075999));
#17170=CARTESIAN_POINT('Ctrl Pts',(-203.301908910968,-62.0373342832907,
9.26858855956428));
#17171=CARTESIAN_POINT('Ctrl Pts',(-206.57081814586,-61.9679327434484,9.4274968783686));
#17172=CARTESIAN_POINT('Ctrl Pts',(-208.399618861337,-64.6782965756237,
9.58640519717289));
#17173=CARTESIAN_POINT('Ctrl Pts',(-207.111687001578,-67.6835945116545,
9.7453135159772));
#17174=CARTESIAN_POINT('Ctrl Pts',(-203.887784100661,-68.2286029933815,
9.90422183478151));
#17175=CARTESIAN_POINT('Ctrl Pts',(-201.683548305251,-65.8136643362045,
10.0631301535858));
#17176=CARTESIAN_POINT('Ctrl Pts',(-202.519798356292,-62.6527673097532,
10.2220384723901));
#17177=CARTESIAN_POINT('Ctrl Pts',(-205.629869553584,-61.6437869791857,
10.3809467911944));
#17178=CARTESIAN_POINT('Ctrl Pts',(-208.162483384071,-63.7117452344017,
10.5398551099987));
#17179=CARTESIAN_POINT('Ctrl Pts',(-207.795767794466,-66.960761060161,10.698763428803));
#17180=CARTESIAN_POINT('Ctrl Pts',(-204.865923538612,-68.4121730609857,
10.8576717476073));
#17181=CARTESIAN_POINT('Ctrl Pts',(-202.058999084014,-66.7353429366515,
11.0165800664117));
#17182=CARTESIAN_POINT('Ctrl Pts',(-201.948351398233,-63.4675698035645,
11.175488385216));
#17183=CARTESIAN_POINT('Ctrl Pts',(-204.635421042906,-61.604711546914,11.3343967040203));
#17184=CARTESIAN_POINT('Ctrl Pts',(-207.656732600619,-62.8546157956158,
11.4933050228246));
#17185=CARTESIAN_POINT('Ctrl Pts',(-208.242381403836,-66.0713843043812,
11.6522133416289));
#17186=CARTESIAN_POINT('Ctrl Pts',(-205.855451175442,-68.3059196575311,
11.8111216604332));
#17187=CARTESIAN_POINT('Ctrl Pts',(-202.684252870604,-67.5096248182363,
11.9700299792375));
#17188=CARTESIAN_POINT('Ctrl Pts',(-201.636105651369,-64.4125339951416,
12.1289382980418));
#17189=CARTESIAN_POINT('Ctrl Pts',(-203.671939173408,-61.8540254393122,
12.2878466168461));
#17190=CARTESIAN_POINT('Ctrl Pts',(-206.925324017804,-62.1797111988197,
12.4467549356504));
#17191=CARTESIAN_POINT('Ctrl Pts',(-208.413593321628,-65.0910062094532,
12.6056632544547));
#17192=CARTESIAN_POINT('Ctrl Pts',(-206.772318421206,-67.9188677444407,
12.764571573259));
#17193=CARTESIAN_POINT('Ctrl Pts',(-203.506201801068,-68.0707439548588,
12.9234798920633));
#17194=CARTESIAN_POINT('Ctrl Pts',(-201.609582673819,-65.4073964286302,
13.0823882108676));
#17195=CARTESIAN_POINT('Ctrl Pts',(-202.821260257257,-62.3705524098184,
13.2412965296719));
#17196=CARTESIAN_POINT('Ctrl Pts',(-206.03038208544,-61.744356553306,13.4002048484763));
#17197=CARTESIAN_POINT('Ctrl Pts',(-208.29486113422,-64.1028982202188,13.5591131672806));
#17198=CARTESIAN_POINT('Ctrl Pts',(-207.538648320798,-67.283892773864,13.7180214860849));
#17199=CARTESIAN_POINT('Ctrl Pts',(-204.455031101497,-68.3710399554251,
13.8769298048892));
#17200=CARTESIAN_POINT('Ctrl Pts',(-201.871035275935,-66.3676553906861,
14.0358381236935));
#17201=CARTESIAN_POINT('Ctrl Pts',(-202.155639340496,-63.1104196344985,
14.1947464424978));
#17202=CARTESIAN_POINT('Ctrl Pts',(-205.047921460904,-61.5855300693876,
14.3536547613021));
#17203=CARTESIAN_POINT('Ctrl Pts',(-207.896269733824,-63.1909883091252,
14.5125630801064));
#17204=CARTESIAN_POINT('Ctrl Pts',(-208.089350260542,-66.4549283813293,
14.6714713989107));
#17205=CARTESIAN_POINT('Ctrl Pts',(-205.450149049385,-68.3850061007028,
14.830379717715));
#17206=CARTESIAN_POINT('Ctrl Pts',(-202.398256114005,-67.2117486250819,
14.9892880365193));
#17207=CARTESIAN_POINT('Ctrl Pts',(-201.731613114368,-64.0107835678785,
15.1481963553236));
#17208=CARTESIAN_POINT('Ctrl Pts',(-204.061390228038,-61.7167234723125,
15.3071046741279));
#17209=CARTESIAN_POINT('Ctrl Pts',(-207.251675223312,-62.4327296745389,
15.4660129929322));
#17210=CARTESIAN_POINT('Ctrl Pts',(-208.377647618961,-65.5023907589485,
15.6249213117365));
#17211=CARTESIAN_POINT('Ctrl Pts',(-206.407034384366,-68.111444732263,15.7838296305409));
#17212=CARTESIAN_POINT('Ctrl Pts',(-203.146459609106,-67.8680039329691,
15.9427379493452));
#17213=CARTESIAN_POINT('Ctrl Pts',(-201.585206711849,-64.9951206969416,
16.1016462681495));
#17214=CARTESIAN_POINT('Ctrl Pts',(-203.15456362261,-62.1268929160954,16.2605545869538));
#17215=CARTESIAN_POINT('Ctrl Pts',(-206.415867028873,-61.8923225795219,
16.4194629057581));
#17216=CARTESIAN_POINT('Ctrl Pts',(-208.378973133268,-64.507608261601,16.5783712245624));
#17217=CARTESIAN_POINT('Ctrl Pts',(-207.244575808431,-67.572723779591,16.7372795433667));
#17218=CARTESIAN_POINT('Ctrl Pts',(-204.051765404813,-68.2824807612099,
16.896187862171));
#17219=CARTESIAN_POINT('Ctrl Pts',(-201.729618763932,-65.9761361990972,
17.0550961809753));
#17220=CARTESIAN_POINT('Ctrl Pts',(-202.180151203454,-63.8537350466212,
17.1610350601782));
#17221=CARTESIAN_POINT('Ctrl Pts',(-202.804802895981,-63.1231365609213,
17.2140044997796));
#17222=CARTESIAN_POINT('Ctrl Pts',(-204.301933573839,-67.6111321859386,
-0.214004499779622));
#17223=CARTESIAN_POINT('Ctrl Pts',(-203.43290490324,-67.378803948562,-0.161035060178186));
#17224=CARTESIAN_POINT('Ctrl Pts',(-201.960375505185,-65.9807910693062,
-0.0550961809753148));
#17225=CARTESIAN_POINT('Ctrl Pts',(-202.528682934436,-62.9711396388145,
0.103812137828991));
#17226=CARTESIAN_POINT('Ctrl Pts',(-205.367277533696,-61.8260315013409,
0.262720456633298));
#17227=CARTESIAN_POINT('Ctrl Pts',(-207.866943113308,-63.5885720031053,
0.421628775437605));
#17228=CARTESIAN_POINT('Ctrl Pts',(-207.739302248069,-66.646159942469,0.580537094241911));
#17229=CARTESIAN_POINT('Ctrl Pts',(-205.099777638078,-68.1940489098917,
0.739445413046219));
#17230=CARTESIAN_POINT('Ctrl Pts',(-202.369031594917,-66.8139210936934,
0.898353731850524));
#17231=CARTESIAN_POINT('Ctrl Pts',(-202.050204799108,-63.7706884983198,
1.05726205065483));
#17232=CARTESIAN_POINT('Ctrl Pts',(-204.435777109006,-61.8545343034827,
1.21617036945914));
#17233=CARTESIAN_POINT('Ctrl Pts',(-207.338593594527,-62.8220790711336,
1.37507868826345));
#17234=CARTESIAN_POINT('Ctrl Pts',(-208.097427728659,-65.7863314092215,
1.53398700706775));
#17235=CARTESIAN_POINT('Ctrl Pts',(-206.016567882626,-68.029677097083,1.69289532587206));
#17236=CARTESIAN_POINT('Ctrl Pts',(-203.003733294953,-67.4954519889176,
1.85180364467637));
#17237=CARTESIAN_POINT('Ctrl Pts',(-201.821052092491,-64.6734227833063,
2.01071196348067));
#17238=CARTESIAN_POINT('Ctrl Pts',(-203.552795587186,-62.1507966995761,
2.16962028228498));
#17239=CARTESIAN_POINT('Ctrl Pts',(-206.611319530648,-62.2402879779792,
2.32852860108929));
#17240=CARTESIAN_POINT('Ctrl Pts',(-208.192603923254,-64.8598525774122,
2.48743691989359));
#17241=CARTESIAN_POINT('Ctrl Pts',(-206.846944632009,-67.6079026781108,
2.6463452386979));
#17242=CARTESIAN_POINT('Ctrl Pts',(-203.808027188815,-67.965056794915,2.80525355750221));
#17243=CARTESIAN_POINT('Ctrl Pts',(-201.861897075226,-65.6038799608823,
2.96416187630651));
#17244=CARTESIAN_POINT('Ctrl Pts',(-202.792744659467,-62.6890727383964,
3.12307019511082));
#17245=CARTESIAN_POINT('Ctrl Pts',(-205.747179264856,-61.8928977956174,
3.28197851391512));
#17246=CARTESIAN_POINT('Ctrl Pts',(-208.01660827373,-63.9452794287941,3.44088683271943));
#17247=CARTESIAN_POINT('Ctrl Pts',(-207.520444532071,-66.9646170920847,
3.59979515152374));
#17248=CARTESIAN_POINT('Ctrl Pts',(-204.713565414472,-68.1828157640413,
3.75870347032805));
#17249=CARTESIAN_POINT('Ctrl Pts',(-202.169286323185,-66.4830445169217,
3.91761178913235));
#17250=CARTESIAN_POINT('Ctrl Pts',(-202.220173892637,-63.4236346325047,
4.07652010793666));
#17251=CARTESIAN_POINT('Ctrl Pts',(-204.819574967711,-61.8094188982323,
4.23542842674097));
#17252=CARTESIAN_POINT('Ctrl Pts',(-207.584387695847,-63.120292257627,4.39433674554527));
#17253=CARTESIAN_POINT('Ctrl Pts',(-207.979862669581,-66.154460666109,4.55324506434958));
#17254=CARTESIAN_POINT('Ctrl Pts',(-205.643432853161,-68.130232439078,4.71215338315389));
#17255=CARTESIAN_POINT('Ctrl Pts',(-202.717110988474,-67.2362420978575,
4.87106170195819));
#17256=CARTESIAN_POINT('Ctrl Pts',(-201.883716254178,-64.2920899953385,
5.0299700207625));
#17257=CARTESIAN_POINT('Ctrl Pts',(-203.907295627992,-61.9969418729286,
5.1888783395668));
#17258=CARTESIAN_POINT('Ctrl Pts',(-206.932654157132,-62.4549638768584,
5.34778665837112));
#17259=CARTESIAN_POINT('Ctrl Pts',(-208.18617695589,-65.2462465531416,5.50669497717542));
#17260=CARTESIAN_POINT('Ctrl Pts',(-206.518648332729,-67.8117731417515,
5.66560329597973));
#17261=CARTESIAN_POINT('Ctrl Pts',(-203.458839891741,-67.7994975406107,
5.82451161478403));
#17262=CARTESIAN_POINT('Ctrl Pts',(-201.811949812777,-65.2206738836432,
5.98341993358834));
#17263=CARTESIAN_POINT('Ctrl Pts',(-203.087828513282,-62.439538876578,6.14232825239265));
#17264=CARTESIAN_POINT('Ctrl Pts',(-206.116764660864,-62.0058060097215,
6.30123657119696));
#17265=CARTESIAN_POINT('Ctrl Pts',(-208.121863449215,-64.3171167276652,
6.46014489000126));
#17266=CARTESIAN_POINT('Ctrl Pts',(-207.264872719747,-67.2544871972402,
6.61905320880557));
#17267=CARTESIAN_POINT('Ctrl Pts',(-204.33147199483,-68.1249690023228,6.77796152760988));
#17268=CARTESIAN_POINT('Ctrl Pts',(-202.010970273053,-66.1305141532081,
6.93686984641418));
#17269=CARTESIAN_POINT('Ctrl Pts',(-202.430777597174,-63.0996165639554,
7.09577816521849));
#17270=CARTESIAN_POINT('Ctrl Pts',(-205.206019304538,-61.8109692686754,
7.25468648402279));
#17271=CARTESIAN_POINT('Ctrl Pts',(-207.792384816137,-63.4459897047368,
7.4135948028271));
#17272=CARTESIAN_POINT('Ctrl Pts',(-207.818723138209,-66.5057094106436,
7.5725031216314));
#17273=CARTESIAN_POINT('Ctrl Pts',(-205.260887591457,-68.1850115578752,
7.73141144043572));
#17274=CARTESIAN_POINT('Ctrl Pts',(-202.463873216744,-66.9443307070625,
7.89031975924001));
#17275=CARTESIAN_POINT('Ctrl Pts',(-201.991951531155,-63.9211091953971,
8.04922807804433));
#17276=CARTESIAN_POINT('Ctrl Pts',(-204.277775061468,-61.8870027148524,
8.20813639684863));
#17277=CARTESIAN_POINT('Ctrl Pts',(-207.225726343268,-62.7068573520037,
8.36704471565294));
#17278=CARTESIAN_POINT('Ctrl Pts',(-208.133156590043,-65.629039538857,8.52595303445725));
#17279=CARTESIAN_POINT('Ctrl Pts',(-206.16814389371,-67.9745253071309,8.68486135326155));
#17280=CARTESIAN_POINT('Ctrl Pts',(-203.132189931727,-67.5929995194816,
8.84376967206586));
#17281=CARTESIAN_POINT('Ctrl Pts',(-201.808623364209,-64.8342407537912,
9.00267799087017));
#17282=CARTESIAN_POINT('Ctrl Pts',(-203.410875227028,-62.227448212368,9.16158630967447));
#17283=CARTESIAN_POINT('Ctrl Pts',(-206.470018920388,-62.162500161608,9.32049462847879));
#17284=CARTESIAN_POINT('Ctrl Pts',(-208.181465697634,-64.6989402485364,
9.47940294728307));
#17285=CARTESIAN_POINT('Ctrl Pts',(-206.976180281873,-67.5113885507243,
9.63831126608739));
#17286=CARTESIAN_POINT('Ctrl Pts',(-203.95915487105,-68.0214238988787,9.7972195848917));
#17287=CARTESIAN_POINT('Ctrl Pts',(-201.896364641136,-65.7614515863713,
9.956127903696));
#17288=CARTESIAN_POINT('Ctrl Pts',(-202.678952619539,-62.8033889700657,
10.1150362225003));
#17289=CARTESIAN_POINT('Ctrl Pts',(-205.589450894481,-61.8591547949365,
10.2739445413046));
#17290=CARTESIAN_POINT('Ctrl Pts',(-207.959547177534,-63.7944123992321,
10.4328528601089));
#17291=CARTESIAN_POINT('Ctrl Pts',(-207.616363686471,-66.8349392413083,
10.5917611789132));
#17292=CARTESIAN_POINT('Ctrl Pts',(-204.874527210207,-68.1932142956896,
10.7506694977175));
#17293=CARTESIAN_POINT('Ctrl Pts',(-202.247722785242,-66.6239861736786,
10.9095778165219));
#17294=CARTESIAN_POINT('Ctrl Pts',(-202.144175349134,-63.5659056785969,
11.0684861353262));
#17295=CARTESIAN_POINT('Ctrl Pts',(-204.658816033978,-61.8225868288017,
11.2273944541305));
#17296=CARTESIAN_POINT('Ctrl Pts',(-207.486250365528,-62.9922848610711,
11.3863027729348));
#17297=CARTESIAN_POINT('Ctrl Pts',(-208.034318150269,-66.0026336928935,
11.5452110917391));
#17298=CARTESIAN_POINT('Ctrl Pts',(-205.800556968789,-68.0937791613008,
11.7041194105434));
#17299=CARTESIAN_POINT('Ctrl Pts',(-202.832854105983,-67.3485824731571,
11.8630277293477));
#17300=CARTESIAN_POINT('Ctrl Pts',(-201.851966377071,-64.4502316232448,
12.021936048152));
#17301=CARTESIAN_POINT('Ctrl Pts',(-203.757160688739,-62.0559022764919,
12.1808443669563));
#17302=CARTESIAN_POINT('Ctrl Pts',(-206.801776190012,-62.3606888170845,
12.3397526857606));
#17303=CARTESIAN_POINT('Ctrl Pts',(-208.194543418365,-65.0851663511284,
12.4986610045649));
#17304=CARTESIAN_POINT('Ctrl Pts',(-206.658588945508,-67.7315643263658,
12.6575693233692));
#17305=CARTESIAN_POINT('Ctrl Pts',(-203.602058665123,-67.8736946572765,
12.8164776421735));
#17306=CARTESIAN_POINT('Ctrl Pts',(-201.827145376036,-65.3812538451784,
12.9753859609778));
#17307=CARTESIAN_POINT('Ctrl Pts',(-202.961069743894,-62.5392837688283,
13.1342942797821));
#17308=CARTESIAN_POINT('Ctrl Pts',(-205.964262581775,-61.9532708306864,
13.2932025985864));
#17309=CARTESIAN_POINT('Ctrl Pts',(-208.083430262199,-64.1604651415136,
13.4521109173907));
#17310=CARTESIAN_POINT('Ctrl Pts',(-207.375743540791,-67.1373356289315,
13.6110192361951));
#17311=CARTESIAN_POINT('Ctrl Pts',(-204.490001695019,-68.1547206969317,
13.7699275549994));
#17312=CARTESIAN_POINT('Ctrl Pts',(-202.071820593793,-66.279893096587,13.9288358738037));
#17313=CARTESIAN_POINT('Ctrl Pts',(-202.338161647229,-63.2316737961026,
14.087744192608));
#17314=CARTESIAN_POINT('Ctrl Pts',(-205.044846346095,-61.8046362245518,
14.2466525114123));
#17315=CARTESIAN_POINT('Ctrl Pts',(-207.710416427574,-63.3070723878518,
14.4055608302166));
#17316=CARTESIAN_POINT('Ctrl Pts',(-207.891106998396,-66.3615657891406,
14.5644691490209));
#17317=CARTESIAN_POINT('Ctrl Pts',(-205.421263035021,-68.1677906362224,
14.7233774678252));
#17318=CARTESIAN_POINT('Ctrl Pts',(-202.565209729402,-67.0698209621416,
14.8822857866295));
#17319=CARTESIAN_POINT('Ctrl Pts',(-201.941345136806,-64.0742614761548,
15.0411941054338));
#17320=CARTESIAN_POINT('Ctrl Pts',(-204.121620712568,-61.9274109614226,
15.2001024242381));
#17321=CARTESIAN_POINT('Ctrl Pts',(-207.10718547501,-62.5974711253967,15.3590107430424));
#17322=CARTESIAN_POINT('Ctrl Pts',(-208.160904347434,-65.4701523999,15.5179190618468));
#17323=CARTESIAN_POINT('Ctrl Pts',(-206.316745144628,-67.9117836703277,
15.6768273806511));
#17324=CARTESIAN_POINT('Ctrl Pts',(-203.265401089553,-67.6839644400115,
15.8357356994554));
#17325=CARTESIAN_POINT('Ctrl Pts',(-201.80433361683,-64.9954338012754,15.9946440182597));
#17326=CARTESIAN_POINT('Ctrl Pts',(-203.272985069414,-62.3112598776802,
16.153552337064));
#17327=CARTESIAN_POINT('Ctrl Pts',(-206.325010999321,-62.0917418934795,
16.3124606558683));
#17328=CARTESIAN_POINT('Ctrl Pts',(-208.162144803636,-64.5392049846145,
16.4713689746726));
#17329=CARTESIAN_POINT('Ctrl Pts',(-207.100541628792,-67.4076323811892,
16.6302772934769));
#17330=CARTESIAN_POINT('Ctrl Pts',(-204.112613513177,-68.0718443363461,
16.7891856122812));
#17331=CARTESIAN_POINT('Ctrl Pts',(-201.939478763615,-65.9134976479173,
16.9480939310855));
#17332=CARTESIAN_POINT('Ctrl Pts',(-202.36110058667,-63.9272907410154,17.0540328102884));
#17333=CARTESIAN_POINT('Ctrl Pts',(-202.945668449658,-63.2435746787732,
17.1070022498898));
#17334=CARTESIAN_POINT('Ctrl Pts',(-204.349800002025,-67.4320868020351,
-0.321006749669433));
#17335=CARTESIAN_POINT('Ctrl Pts',(-203.540360643981,-67.2156893163365,
-0.268037310067997));
#17336=CARTESIAN_POINT('Ctrl Pts',(-202.168802614899,-65.9135382069353,
-0.162098430865125));
#17337=CARTESIAN_POINT('Ctrl Pts',(-202.698141192863,-63.1102586325642,
-0.00319011206081941));
#17338=CARTESIAN_POINT('Ctrl Pts',(-205.34209330619,-62.0436705819667,0.155718206743488));
#17339=CARTESIAN_POINT('Ctrl Pts',(-207.670356769225,-63.6853536478328,
0.314626525547794));
#17340=CARTESIAN_POINT('Ctrl Pts',(-207.551468240555,-66.5332827237463,
0.473534844352101));
#17341=CARTESIAN_POINT('Ctrl Pts',(-205.092935883528,-67.9750329150838,
0.632443163156408));
#17342=CARTESIAN_POINT('Ctrl Pts',(-202.549437148746,-66.6895404896243,
0.791351481960714));
#17343=CARTESIAN_POINT('Ctrl Pts',(-202.25247231242,-63.8549824114892,0.95025980076502));
#17344=CARTESIAN_POINT('Ctrl Pts',(-204.474465883427,-62.0702189464208,
1.10916811956933));
#17345=CARTESIAN_POINT('Ctrl Pts',(-207.178236187047,-62.9714191508586,
1.26807643837363));
#17346=CARTESIAN_POINT('Ctrl Pts',(-207.885037050096,-65.7324126494599,
1.42698475717794));
#17347=CARTESIAN_POINT('Ctrl Pts',(-205.946861803482,-67.8219320806215,
1.58589307598225));
#17348=CARTESIAN_POINT('Ctrl Pts',(-203.140617341079,-67.324338798335,1.74480139478656));
#17349=CARTESIAN_POINT('Ctrl Pts',(-202.039032611277,-64.6958161892978,
1.90370971359086));
#17350=CARTESIAN_POINT('Ctrl Pts',(-203.652030421438,-62.3461666243507,
2.06261803239517));
#17351=CARTESIAN_POINT('Ctrl Pts',(-206.50083131963,-62.4295214840832,2.22152635119947));
#17352=CARTESIAN_POINT('Ctrl Pts',(-207.973687011208,-64.869462488858,2.38043467000378));
#17353=CARTESIAN_POINT('Ctrl Pts',(-206.720299603286,-67.4290787416208,
2.53934298880809));
#17354=CARTESIAN_POINT('Ctrl Pts',(-203.889760787264,-67.7617427938084,
2.6982513076124));
#17355=CARTESIAN_POINT('Ctrl Pts',(-202.077076852765,-65.5624719004209,
2.8571596264167));
#17356=CARTESIAN_POINT('Ctrl Pts',(-202.944096200361,-62.8475330648997,
3.01606794522101));
#17357=CARTESIAN_POINT('Ctrl Pts',(-205.695945168382,-62.1059518531665,
3.17497626402531));
#17358=CARTESIAN_POINT('Ctrl Pts',(-207.809759386736,-64.0176016385234,
3.33388458282963));
#17359=CARTESIAN_POINT('Ctrl Pts',(-207.347617602327,-66.8299032605253,
3.49279290163393));
#17360=CARTESIAN_POINT('Ctrl Pts',(-204.733206239477,-67.9645700262592,
3.65170122043824));
#17361=CARTESIAN_POINT('Ctrl Pts',(-202.363388414116,-66.3813521260468,
3.81060953924254));
#17362=CARTESIAN_POINT('Ctrl Pts',(-202.410786621957,-63.5317260358873,
3.96951785804685));
#17363=CARTESIAN_POINT('Ctrl Pts',(-204.831946715624,-62.0281971053708,
4.12842617685115));
#17364=CARTESIAN_POINT('Ctrl Pts',(-207.40717618214,-63.2491838534535,4.28733449565546));
#17365=CARTESIAN_POINT('Ctrl Pts',(-207.775533429366,-66.0752992761655,
4.44624281445977));
#17366=CARTESIAN_POINT('Ctrl Pts',(-205.59931265012,-67.9155923408937,4.60515113326408));
#17367=CARTESIAN_POINT('Ctrl Pts',(-202.873648731634,-67.0829029344599,
4.76405945206838));
#17368=CARTESIAN_POINT('Ctrl Pts',(-202.097399890199,-64.3406313978904,
4.92296777087269));
#17369=CARTESIAN_POINT('Ctrl Pts',(-203.982222387668,-62.2028616261076,
5.08187608967699));
#17370=CARTESIAN_POINT('Ctrl Pts',(-206.800132024633,-62.6294770524725,
5.2407844084813));
#17371=CARTESIAN_POINT('Ctrl Pts',(-207.967700741118,-65.2293614222855,
5.39969272728561));
#17372=CARTESIAN_POINT('Ctrl Pts',(-206.414514587523,-67.6189698036725,
5.55860104608992));
#17373=CARTESIAN_POINT('Ctrl Pts',(-203.564517269825,-67.6075359407365,
5.71750936489422));
#17374=CARTESIAN_POINT('Ctrl Pts',(-202.030554475057,-65.2055422712234,
5.87641768369853));
#17375=CARTESIAN_POINT('Ctrl Pts',(-203.218946148679,-62.6151097447562,
6.03532600250284));
#17376=CARTESIAN_POINT('Ctrl Pts',(-206.040188086721,-62.2111179488711,
6.19423432130714));
#17377=CARTESIAN_POINT('Ctrl Pts',(-207.907797212825,-64.363942046703,6.35314264011145));
#17378=CARTESIAN_POINT('Ctrl Pts',(-207.109570354059,-67.0998969670293,
6.51205095891575));
#17379=CARTESIAN_POINT('Ctrl Pts',(-204.377312972924,-67.9106898180974,
6.67095927772007));
#17380=CARTESIAN_POINT('Ctrl Pts',(-202.215928098567,-66.0529947761121,
6.82986759652436));
#17381=CARTESIAN_POINT('Ctrl Pts',(-202.606949226449,-63.2299258924922,
6.98877591532868));
#17382=CARTESIAN_POINT('Ctrl Pts',(-205.191892556888,-62.0296411668831,
7.14768423413298));
#17383=CARTESIAN_POINT('Ctrl Pts',(-207.600910935916,-63.552548220389,7.30659255293729));
#17384=CARTESIAN_POINT('Ctrl Pts',(-207.62544323874,-66.4024628875731,7.46550087174159));
#17385=CARTESIAN_POINT('Ctrl Pts',(-205.242998524324,-67.9666152544678,
7.6244091905459));
#17386=CARTESIAN_POINT('Ctrl Pts',(-202.637775478752,-66.8110079133119,
7.78331750935021));
#17387=CARTESIAN_POINT('Ctrl Pts',(-202.198213472165,-63.9950887584926,
7.94222582815451));
#17388=CARTESIAN_POINT('Ctrl Pts',(-204.327298039309,-62.1004609982022,
8.10113414695882));
#17389=CARTESIAN_POINT('Ctrl Pts',(-207.073108245363,-62.864098187212,8.26004246576313));
#17390=CARTESIAN_POINT('Ctrl Pts',(-207.918315982771,-65.5859062856529,
8.41895078456743));
#17391=CARTESIAN_POINT('Ctrl Pts',(-206.088044244589,-67.7705620499607,
8.57785910337174));
#17392=CARTESIAN_POINT('Ctrl Pts',(-203.260265703813,-67.4151974928637,
8.73676742217605));
#17393=CARTESIAN_POINT('Ctrl Pts',(-202.027456121131,-64.8456068684723,
8.89567574098036));
#17394=CARTESIAN_POINT('Ctrl Pts',(-203.519841543088,-62.4175621414454,
9.05458405978466));
#17395=CARTESIAN_POINT('Ctrl Pts',(-206.369219694917,-62.3570675797674,
9.21349237858898));
#17396=CARTESIAN_POINT('Ctrl Pts',(-207.963312533931,-64.7195839214493,
9.37240069739327));
#17397=CARTESIAN_POINT('Ctrl Pts',(-206.840673562169,-67.3391825897941,
9.53130901619758));
#17398=CARTESIAN_POINT('Ctrl Pts',(-204.030525641438,-67.8142448043757,
9.69021733500189));
#17399=CARTESIAN_POINT('Ctrl Pts',(-202.109180977022,-65.7092388365381,
9.84912565380619));
#17400=CARTESIAN_POINT('Ctrl Pts',(-202.838106882786,-62.9540106303781,
10.0080339726105));
#17401=CARTESIAN_POINT('Ctrl Pts',(-205.549032235379,-62.0745226106873,
10.1669422914148));
#17402=CARTESIAN_POINT('Ctrl Pts',(-207.756610970996,-63.8770795640624,
10.3258506102191));
#17403=CARTESIAN_POINT('Ctrl Pts',(-207.436959578475,-66.7091174224556,
10.4847589290234));
#17404=CARTESIAN_POINT('Ctrl Pts',(-204.883130881801,-67.9742555303935,
10.6436672478277));
#17405=CARTESIAN_POINT('Ctrl Pts',(-202.43644648647,-66.5126294107058,10.802575566632));
#17406=CARTESIAN_POINT('Ctrl Pts',(-202.339999300035,-63.6642415536293,
10.9614838854363));
#17407=CARTESIAN_POINT('Ctrl Pts',(-204.68221102505,-62.0404621106893,11.1203922042406));
#17408=CARTESIAN_POINT('Ctrl Pts',(-207.315768130438,-63.1299539265266,
11.279300523045));
#17409=CARTESIAN_POINT('Ctrl Pts',(-207.826254896701,-65.9338830814056,
11.4382088418493));
#17410=CARTESIAN_POINT('Ctrl Pts',(-205.745662762136,-67.8816386650706,
11.5971171606536));
#17411=CARTESIAN_POINT('Ctrl Pts',(-202.981455341363,-67.1875401280777,
11.7560254794579));
#17412=CARTESIAN_POINT('Ctrl Pts',(-202.067827102772,-64.4879292513482,
11.9149337982622));
#17413=CARTESIAN_POINT('Ctrl Pts',(-203.84238220407,-62.2577791136714,12.0738421170665));
#17414=CARTESIAN_POINT('Ctrl Pts',(-206.678228362221,-62.5416664353495,
12.2327504358708));
#17415=CARTESIAN_POINT('Ctrl Pts',(-207.975493515101,-65.0793264928035,
12.3916587546751));
#17416=CARTESIAN_POINT('Ctrl Pts',(-206.544859469809,-67.5442609082911,
12.5505670734794));
#17417=CARTESIAN_POINT('Ctrl Pts',(-203.697915529178,-67.6766453596943,
12.7094753922837));
#17418=CARTESIAN_POINT('Ctrl Pts',(-202.044708078252,-65.3551112617265,
12.868383711088));
#17419=CARTESIAN_POINT('Ctrl Pts',(-203.100879230531,-62.7080151278382,
13.0272920298923));
#17420=CARTESIAN_POINT('Ctrl Pts',(-205.89814307811,-62.1621851080667,13.1862003486966));
#17421=CARTESIAN_POINT('Ctrl Pts',(-207.871999390178,-64.2180320628083,
13.3451086675009));
#17422=CARTESIAN_POINT('Ctrl Pts',(-207.212838760785,-66.9907784839988,
13.5040169863053));
#17423=CARTESIAN_POINT('Ctrl Pts',(-204.52497228854,-67.9384014384382,13.6629253051096));
#17424=CARTESIAN_POINT('Ctrl Pts',(-202.272605911651,-66.192130802488,13.8218336239139));
#17425=CARTESIAN_POINT('Ctrl Pts',(-202.520683953961,-63.3529279577067,
13.9807419427182));
#17426=CARTESIAN_POINT('Ctrl Pts',(-205.041771231286,-62.0237423797161,
14.1396502615225));
#17427=CARTESIAN_POINT('Ctrl Pts',(-207.524563121323,-63.4231564665784,
14.2985585803268));
#17428=CARTESIAN_POINT('Ctrl Pts',(-207.692863736251,-66.2682031969519,
14.4574668991311));
#17429=CARTESIAN_POINT('Ctrl Pts',(-205.392377020657,-67.9505751717419,
14.6163752179354));
#17430=CARTESIAN_POINT('Ctrl Pts',(-202.7321633448,-66.9278932992014,14.7752835367397));
#17431=CARTESIAN_POINT('Ctrl Pts',(-202.151077159244,-64.137739384431,14.934191855544));
#17432=CARTESIAN_POINT('Ctrl Pts',(-204.181851197098,-62.1380984505328,
15.0931001743483));
#17433=CARTESIAN_POINT('Ctrl Pts',(-206.962695726708,-62.7622125762542,
15.2520084931526));
#17434=CARTESIAN_POINT('Ctrl Pts',(-207.944161075907,-65.4379140408516,
15.4109168119569));
#17435=CARTESIAN_POINT('Ctrl Pts',(-206.226455904891,-67.7121226083924,
15.5698251307612));
#17436=CARTESIAN_POINT('Ctrl Pts',(-203.38434257,-67.499924947054,15.7287334495656));
#17437=CARTESIAN_POINT('Ctrl Pts',(-202.023460521812,-64.9957469056093,
15.8876417683698));
#17438=CARTESIAN_POINT('Ctrl Pts',(-203.391406516217,-62.4956268392649,
16.0465500871742));
#17439=CARTESIAN_POINT('Ctrl Pts',(-206.234154969769,-62.2911612074372,
16.2054584059785));
#17440=CARTESIAN_POINT('Ctrl Pts',(-207.945316474004,-64.5708017076279,
16.3643667247828));
#17441=CARTESIAN_POINT('Ctrl Pts',(-206.956507449152,-67.2425409827873,
16.5232750435871));
#17442=CARTESIAN_POINT('Ctrl Pts',(-204.173461621541,-67.8612079114822,
16.6821833623914));
#17443=CARTESIAN_POINT('Ctrl Pts',(-202.149338763299,-65.8508590967375,
16.8410916811957));
#17444=CARTESIAN_POINT('Ctrl Pts',(-202.542049969887,-64.0008464354096,
16.9470305603986));
#17445=CARTESIAN_POINT('Ctrl Pts',(-203.086534003335,-63.3640127966251,
17.));
#17446=CARTESIAN_POINT('Ctrl Pts',(-202.485823045017,-64.9986459985219,
0.88741669750801));
#17447=CARTESIAN_POINT('Ctrl Pts',(-202.484195117705,-64.6662426784437,
0.90836439859368));
#17448=CARTESIAN_POINT('Ctrl Pts',(-202.545417607547,-64.3344135715533,
0.92931209967935));
#17449=CARTESIAN_POINT('Ctrl Pts',(-202.672298713642,-64.0299481803337,
0.95025980076502));
#17450=CARTESIAN_POINT('Ctrl Pts',(-202.993136836089,-63.2600612564664,
1.00322924036646));
#17451=CARTESIAN_POINT('Ctrl Pts',(-203.733801359758,-62.6651401014436,
1.05619867996789));
#17452=CARTESIAN_POINT('Ctrl Pts',(-204.554762005529,-62.5178795580052,
1.10916811956933));
#17453=CARTESIAN_POINT('Ctrl Pts',(-205.3757226513,-62.3706190145667,1.16213755917076));
#17454=CARTESIAN_POINT('Ctrl Pts',(-206.276979419173,-62.6710190827126,
1.2151069987722));
#17455=CARTESIAN_POINT('Ctrl Pts',(-206.845407946952,-63.2813846998858,
1.26807643837363));
#17456=CARTESIAN_POINT('Ctrl Pts',(-207.41383647473,-63.891750317059,1.32104587797507));
#17457=CARTESIAN_POINT('Ctrl Pts',(-207.649436762413,-64.8120814832594,
1.37401531757651));
#17458=CARTESIAN_POINT('Ctrl Pts',(-207.444207698485,-65.6205003048866,
1.42698475717794));
#17459=CARTESIAN_POINT('Ctrl Pts',(-207.238978634558,-66.4289191265138,
1.47995419677938));
#17460=CARTESIAN_POINT('Ctrl Pts',(-206.59292021902,-67.1254256035676,1.53292363638081));
#17461=CARTESIAN_POINT('Ctrl Pts',(-205.80218360085,-67.3907466283802,1.58589307598225));
#17462=CARTESIAN_POINT('Ctrl Pts',(-205.011446982681,-67.6560676531927,
1.63886251558368));
#17463=CARTESIAN_POINT('Ctrl Pts',(-204.07603216188,-67.4902032257639,1.69183195518512));
#17464=CARTESIAN_POINT('Ctrl Pts',(-203.424727296512,-66.9691839105433,
1.74480139478655));
#17465=CARTESIAN_POINT('Ctrl Pts',(-202.840201318028,-66.5015851849195,
1.79233982902704));
#17466=CARTESIAN_POINT('Ctrl Pts',(-202.484511916232,-65.7479266885556,
1.83987826326752));
#17467=CARTESIAN_POINT('Ctrl Pts',(-202.479332426993,-64.9985362476049,
1.88741669750801));
#17468=CARTESIAN_POINT('Ctrl Pts',(-204.206200717467,-67.9692229537457,
-8.32667268468867E-16));
#17469=CARTESIAN_POINT('Ctrl Pts',(-204.113162270877,-67.935189074383,-8.43666019689578E-16));
#17470=CARTESIAN_POINT('Ctrl Pts',(-204.022191224303,-67.8963833673696,
-7.93411407245791E-16));
#17471=CARTESIAN_POINT('Ctrl Pts',(-203.933495016826,-67.8531352315209,
-8.39606162372775E-16));
#17472=CARTESIAN_POINT('Ctrl Pts',(-203.84282083649,-67.8089226391153,-8.86831085242262E-16));
#17473=CARTESIAN_POINT('Ctrl Pts',(-203.754523420144,-67.7600666539124,
-9.43046358883727E-16));
#17474=CARTESIAN_POINT('Ctrl Pts',(-203.668853328449,-67.706873635749,-9.61036805691151E-16));
#17475=CARTESIAN_POINT('Ctrl Pts',(-203.585825222369,-67.6553210405853,
-9.78472443921523E-16));
#17476=CARTESIAN_POINT('Ctrl Pts',(-203.505264559179,-67.599693926327,-6.24341674353395E-16));
#17477=CARTESIAN_POINT('Ctrl Pts',(-203.427433248919,-67.5402403758356,
-5.27355936696949E-16));
#17478=CARTESIAN_POINT('Ctrl Pts',(-203.359330852442,-67.4882185191557,
-4.42493416247559E-16));
#17479=CARTESIAN_POINT('Ctrl Pts',(-203.293318414644,-67.4332663265531,
-7.68735084580293E-16));
#17480=CARTESIAN_POINT('Ctrl Pts',(-203.229596756254,-67.3755369799182,
-7.56339435525888E-16));
#17481=CARTESIAN_POINT('Ctrl Pts',(-203.216348808853,-67.3635348543143,
-7.53762338337633E-16));
#17482=CARTESIAN_POINT('Ctrl Pts',(-203.203198226301,-67.3514108995448,
-7.71802573975562E-16));
#17483=CARTESIAN_POINT('Ctrl Pts',(-203.190163693746,-67.3391825254392,
-7.63278329429795E-16));
#17484=CARTESIAN_POINT('Ctrl Pts',(-203.117740153311,-67.2712382287989,
-7.15915221706024E-16));
#17485=CARTESIAN_POINT('Ctrl Pts',(-203.048782419931,-67.1999720891002,
-1.01902361823498E-15));
#17486=CARTESIAN_POINT('Ctrl Pts',(-202.983529622551,-67.1256761154066,
-1.06858966120171E-15));
#17487=CARTESIAN_POINT('Ctrl Pts',(-202.918635398475,-67.0517884085421,
-1.11788333178828E-15));
#17488=CARTESIAN_POINT('Ctrl Pts',(-202.857405018863,-66.9749032753298,
-6.33633973634577E-16));
#17489=CARTESIAN_POINT('Ctrl Pts',(-202.800117313271,-66.8952811970425,
-6.52256026967279E-16));
#17490=CARTESIAN_POINT('Ctrl Pts',(-202.744165816032,-66.8175162656787,
-6.7044372980576E-16));
#17491=CARTESIAN_POINT('Ctrl Pts',(-202.691974930395,-66.7371398344541,
-1.00351063719331E-15));
#17492=CARTESIAN_POINT('Ctrl Pts',(-202.643851583745,-66.6543804051971,
-9.85322934354826E-16));
#17493=CARTESIAN_POINT('Ctrl Pts',(-202.623072237245,-66.6186454246452,
-9.77469603162805E-16));
#17494=CARTESIAN_POINT('Ctrl Pts',(-202.603051895676,-66.5824660271048,
-9.98257832788744E-16));
#17495=CARTESIAN_POINT('Ctrl Pts',(-202.583818283756,-66.5458602757777,
-9.85322934354826E-16));
#17496=CARTESIAN_POINT('Ctrl Pts',(-202.569903871651,-66.5193781198792,
-9.75965279220305E-16));
#17497=CARTESIAN_POINT('Ctrl Pts',(-202.556401247797,-66.4926728201715,
-7.49717931409916E-16));
#17498=CARTESIAN_POINT('Ctrl Pts',(-202.543321546688,-66.4657512130594,
-7.21644966006352E-16));
#17499=CARTESIAN_POINT('Ctrl Pts',(-202.537160136435,-66.4530693432883,
-7.08420729806322E-16));
#17500=CARTESIAN_POINT('Ctrl Pts',(-202.531094761039,-66.4403438700637,
-5.91077345936009E-16));
#17501=CARTESIAN_POINT('Ctrl Pts',(-202.525129585519,-66.4275826355722,
-5.96744875736022E-16));
#17502=CARTESIAN_POINT('Ctrl Pts',(-202.485113226786,-66.3419760787267,
-6.34764529110435E-16));
#17503=CARTESIAN_POINT('Ctrl Pts',(-202.449555099265,-66.2546652571579,
-7.35539575560742E-16));
#17504=CARTESIAN_POINT('Ctrl Pts',(-202.418706921757,-66.1658877660811,
-6.38378239159465E-16));
#17505=CARTESIAN_POINT('Ctrl Pts',(-202.38854293449,-66.0790792954752,-5.4337187084792E-16));
#17506=CARTESIAN_POINT('Ctrl Pts',(-202.362882072143,-65.9908678196851,
-9.23815234263263E-16));
#17507=CARTESIAN_POINT('Ctrl Pts',(-202.342008857865,-65.9014669200007,
-9.99200722162641E-16));
#17508=CARTESIAN_POINT('Ctrl Pts',(-202.338628864872,-65.8869902605616,
-1.01140787039958E-15));
#17509=CARTESIAN_POINT('Ctrl Pts',(-202.335374520679,-65.8724824066537,
-1.33627779352685E-15));
#17510=CARTESIAN_POINT('Ctrl Pts',(-202.332247164121,-65.8579442614285,
-1.36002320516582E-15));
#17511=CARTESIAN_POINT('Ctrl Pts',(-202.312208856065,-65.7647921608561,
-1.54206868173359E-15));
#17512=CARTESIAN_POINT('Ctrl Pts',(-202.297379937046,-65.6703953939466,
-1.18629651745573E-15));
#17513=CARTESIAN_POINT('Ctrl Pts',(-202.287681809579,-65.5751623462816,
-1.11022302462516E-15));
#17514=CARTESIAN_POINT('Ctrl Pts',(-202.284326013292,-65.5422093139731,
-1.08389968069644E-15));
#17515=CARTESIAN_POINT('Ctrl Pts',(-202.281584984168,-65.5091562792113,
-4.63048300924823E-16));
#17516=CARTESIAN_POINT('Ctrl Pts',(-202.279456820056,-65.4760206859389,
-4.16333634234434E-16));
#17517=CARTESIAN_POINT('Ctrl Pts',(-202.278429738568,-65.4600289895105,
-3.93788488827538E-16));
#17518=CARTESIAN_POINT('Ctrl Pts',(-202.277545413196,-65.4440180689878,
-4.83296287894591E-16));
#17519=CARTESIAN_POINT('Ctrl Pts',(-202.276803684951,-65.4279899164929,
-4.71844785465692E-16));
#17520=CARTESIAN_POINT('Ctrl Pts',(-202.276227068944,-65.4155297070277,
-4.62942441979656E-16));
#17521=CARTESIAN_POINT('Ctrl Pts',(-202.275736729878,-65.4030602298859,
-7.24983344813615E-16));
#17522=CARTESIAN_POINT('Ctrl Pts',(-202.2753327434,-65.3905923140717,-7.21644966006352E-16));
#17523=CARTESIAN_POINT('Ctrl Pts',(-202.272313671571,-65.2974170829925,
-6.96696592803443E-16));
#17524=CARTESIAN_POINT('Ctrl Pts',(-202.2741053936,-65.2041782507755,-5.18105779583049E-16));
#17525=CARTESIAN_POINT('Ctrl Pts',(-202.280568206079,-65.1112502594295,
-6.10622663543836E-16));
#17526=CARTESIAN_POINT('Ctrl Pts',(-202.287044515393,-65.0181281987396,
-7.03332758298409E-16));
#17527=CARTESIAN_POINT('Ctrl Pts',(-202.298211829298,-64.9253172978478,
-8.84079863654896E-16));
#17528=CARTESIAN_POINT('Ctrl Pts',(-202.313980641549,-64.8332063229902,
-8.04911692853238E-16));
#17529=CARTESIAN_POINT('Ctrl Pts',(-202.32952814569,-64.7423880837798,-7.26854611329152E-16));
#17530=CARTESIAN_POINT('Ctrl Pts',(-202.349549362971,-64.6522494151919,
-6.30136933924858E-16));
#17531=CARTESIAN_POINT('Ctrl Pts',(-202.374001579135,-64.5631880635913,
-6.10622663543836E-16));
#17532=CARTESIAN_POINT('Ctrl Pts',(-202.383514240645,-64.5285404682246,
-6.03031014283114E-16));
#17533=CARTESIAN_POINT('Ctrl Pts',(-202.393697939845,-64.4940562580039,
-8.08693639224482E-16));
#17534=CARTESIAN_POINT('Ctrl Pts',(-202.404551732242,-64.4597603152699,
-8.32667268468867E-16));
#17535=CARTESIAN_POINT('Ctrl Pts',(-202.410350756828,-64.4414364881864,
-8.45476032474648E-16));
#17536=CARTESIAN_POINT('Ctrl Pts',(-202.416341081224,-64.4231664197207,
-4.41954415849099E-16));
#17537=CARTESIAN_POINT('Ctrl Pts',(-202.422522657021,-64.4049540190092,
-4.44089209850063E-16));
#17538=CARTESIAN_POINT('Ctrl Pts',(-202.428041258764,-64.3886948984179,
-4.45995047177558E-16));
#17539=CARTESIAN_POINT('Ctrl Pts',(-202.433712830842,-64.3724804931878,
-1.04911529577836E-15));
#17540=CARTESIAN_POINT('Ctrl Pts',(-202.439531012802,-64.3563305530537,
-1.08246744900953E-15));
#17541=CARTESIAN_POINT('Ctrl Pts',(-202.47036464237,-64.2707434615647,-1.25921818407324E-15));
#17542=CARTESIAN_POINT('Ctrl Pts',(-202.505348632287,-64.1868546674516,
-1.34967217968898E-15));
#17543=CARTESIAN_POINT('Ctrl Pts',(-202.544418706298,-64.105044870123,-9.99200722162641E-16));
#17544=CARTESIAN_POINT('Ctrl Pts',(-202.57588160692,-64.0391639218935,-7.16968120406447E-16));
#17545=CARTESIAN_POINT('Ctrl Pts',(-202.60999524185,-63.9746315046024,-1.14052024783077E-15));
#17546=CARTESIAN_POINT('Ctrl Pts',(-202.646744245718,-63.911664139129,-1.38777878078145E-15));
#17547=CARTESIAN_POINT('Ctrl Pts',(-202.661986529103,-63.8855473379223,
-1.49033352327672E-15));
#17548=CARTESIAN_POINT('Ctrl Pts',(-202.677682360038,-63.859699991663,-9.26822014599923E-16));
#17549=CARTESIAN_POINT('Ctrl Pts',(-202.693831375288,-63.8341385429959,
-9.43689570931383E-16));
#17550=CARTESIAN_POINT('Ctrl Pts',(-202.702298017956,-63.8207371281978,
-9.52532931962022E-16));
#17551=CARTESIAN_POINT('Ctrl Pts',(-202.710887811084,-63.8074166610173,
-1.22761254702973E-15));
#17552=CARTESIAN_POINT('Ctrl Pts',(-202.719595895668,-63.7941863862979,
-1.22124532708767E-15));
#17553=CARTESIAN_POINT('Ctrl Pts',(-202.767005235546,-63.7221569308133,
-1.18658033372179E-15));
#17554=CARTESIAN_POINT('Ctrl Pts',(-202.817957036884,-63.6527358475527,
-4.93484857439899E-16));
#17555=CARTESIAN_POINT('Ctrl Pts',(-202.872414575612,-63.5862784909644,
-5.55111512312578E-16));
#17556=CARTESIAN_POINT('Ctrl Pts',(-202.92687211434,-63.5198211343761,-6.16738167185258E-16));
#17557=CARTESIAN_POINT('Ctrl Pts',(-202.984835721377,-63.4563268124908,
-5.65027584124604E-16));
#17558=CARTESIAN_POINT('Ctrl Pts',(-203.046298166971,-63.3961948799941,
-6.66133814775094E-16));
#17559=CARTESIAN_POINT('Ctrl Pts',(-203.058348982186,-63.3844049357444,
-6.85768708283518E-16));
#17560=CARTESIAN_POINT('Ctrl Pts',(-203.070534385631,-63.3727444059762,
-1.54261645251009E-16));
#17561=CARTESIAN_POINT('Ctrl Pts',(-203.082851793447,-63.3612143523573,
-1.66533453693773E-16));
#17562=CARTESIAN_POINT('Origin',(-205.,-65.,9.));
#17563=CARTESIAN_POINT('Origin',(-205.,65.,17.));
#17564=CARTESIAN_POINT('Ctrl Pts',(-203.086534003335,66.6359872033749,17.));
#17565=CARTESIAN_POINT('Ctrl Pts',(-203.024405959645,66.5776020979941,17.));
#17566=CARTESIAN_POINT('Ctrl Pts',(-202.965656494088,66.5159622835985,17.));
#17567=CARTESIAN_POINT('Ctrl Pts',(-202.910296236763,66.4514444609274,17.));
#17568=CARTESIAN_POINT('Ctrl Pts',(-202.853578930092,66.3853451089548,17.));
#17569=CARTESIAN_POINT('Ctrl Pts',(-202.800418561819,66.3162244307376,17.));
#17570=CARTESIAN_POINT('Ctrl Pts',(-202.750855500683,66.2444412342179,17.));
#17571=CARTESIAN_POINT('Ctrl Pts',(-202.737942217452,66.2257386616427,17.));
#17572=CARTESIAN_POINT('Ctrl Pts',(-202.725273298507,66.2068551349331,17.));
#17573=CARTESIAN_POINT('Ctrl Pts',(-202.71284983158,66.1877965690358,17.));
#17574=CARTESIAN_POINT('Ctrl Pts',(-202.702648131353,66.1721463663022,17.));
#17575=CARTESIAN_POINT('Ctrl Pts',(-202.692611475546,66.1563771828948,17.));
#17576=CARTESIAN_POINT('Ctrl Pts',(-202.682749390262,66.1405070166588,17.));
#17577=CARTESIAN_POINT('Ctrl Pts',(-202.635317887944,66.064179768932,17.));
#17578=CARTESIAN_POINT('Ctrl Pts',(-202.59187115121,65.9854441421124,17.));
#17579=CARTESIAN_POINT('Ctrl Pts',(-202.552442406189,65.9046931376478,17.));
#17580=CARTESIAN_POINT('Ctrl Pts',(-202.520315548909,65.838896572369,17.));
#17581=CARTESIAN_POINT('Ctrl Pts',(-202.49085676949,65.7717608847253,17.));
#17582=CARTESIAN_POINT('Ctrl Pts',(-202.464101805081,65.7034802673812,17.));
#17583=CARTESIAN_POINT('Ctrl Pts',(-202.455215975848,65.6808029841515,17.));
#17584=CARTESIAN_POINT('Ctrl Pts',(-202.44662852597,65.6579992976328,17.));
#17585=CARTESIAN_POINT('Ctrl Pts',(-202.438341197581,65.635076009318,17.));
#17586=CARTESIAN_POINT('Ctrl Pts',(-202.431659305257,65.6165934613812,17.));
#17587=CARTESIAN_POINT('Ctrl Pts',(-202.425171725505,65.5980304421231,17.));
#17588=CARTESIAN_POINT('Ctrl Pts',(-202.418887047983,65.5794139527973,17.));
#17589=CARTESIAN_POINT('Ctrl Pts',(-202.38936981961,65.4919779363867,17.));
#17590=CARTESIAN_POINT('Ctrl Pts',(-202.364286281244,65.4032613105746,17.));
#17591=CARTESIAN_POINT('Ctrl Pts',(-202.343667590228,65.3136623471474,17.));
#17592=CARTESIAN_POINT('Ctrl Pts',(-202.322591143159,65.2220741949864,17.));
#17593=CARTESIAN_POINT('Ctrl Pts',(-202.306179437392,65.12956330341,17.));
#17594=CARTESIAN_POINT('Ctrl Pts',(-202.294508583617,65.0365211410702,17.));
#17595=CARTESIAN_POINT('Ctrl Pts',(-202.283004950542,64.9448120924728,17.));
#17596=CARTESIAN_POINT('Ctrl Pts',(-202.276106995875,64.8525859269892,17.));
#17597=CARTESIAN_POINT('Ctrl Pts',(-202.273934698214,64.7601983422578,17.));
#17598=CARTESIAN_POINT('Ctrl Pts',(-202.272809661586,64.7123506560533,17.));
#17599=CARTESIAN_POINT('Ctrl Pts',(-202.272952952458,64.6644594453727,17.));
#17600=CARTESIAN_POINT('Ctrl Pts',(-202.27438671825,64.6165733453971,17.));
#17601=CARTESIAN_POINT('Ctrl Pts',(-202.275036414498,64.5948742508328,17.));
#17602=CARTESIAN_POINT('Ctrl Pts',(-202.275951668491,64.5731691349364,17.));
#17603=CARTESIAN_POINT('Ctrl Pts',(-202.277132318497,64.5515006305554,17.));
#17604=CARTESIAN_POINT('Ctrl Pts',(-202.282342225116,64.4558830606592,17.));
#17605=CARTESIAN_POINT('Ctrl Pts',(-202.292716069493,64.3608730697258,17.));
#17606=CARTESIAN_POINT('Ctrl Pts',(-202.308320883029,64.2668677599894,17.));
#17607=CARTESIAN_POINT('Ctrl Pts',(-202.312169901591,64.2436808003145,17.));
#17608=CARTESIAN_POINT('Ctrl Pts',(-202.316337397629,64.2205548712098,17.));
#17609=CARTESIAN_POINT('Ctrl Pts',(-202.320824840019,64.1974957764614,17.));
#17610=CARTESIAN_POINT('Ctrl Pts',(-202.33832966782,64.1075457675858,17.));
#17611=CARTESIAN_POINT('Ctrl Pts',(-202.360698767987,64.0186128346896,17.));
#17612=CARTESIAN_POINT('Ctrl Pts',(-202.387628946164,63.9309270453222,17.));
#17613=CARTESIAN_POINT('Ctrl Pts',(-202.415161416494,63.8412801674492,17.));
#17614=CARTESIAN_POINT('Ctrl Pts',(-202.447461481234,63.7529361397536,17.));
#17615=CARTESIAN_POINT('Ctrl Pts',(-202.484259321795,63.6661452513196,17.));
#17616=CARTESIAN_POINT('Ctrl Pts',(-202.498888428792,63.6316412376634,17.));
#17617=CARTESIAN_POINT('Ctrl Pts',(-202.514228975924,63.5973828031145,17.));
#17618=CARTESIAN_POINT('Ctrl Pts',(-202.530266183054,63.5633862551367,17.));
#17619=CARTESIAN_POINT('Ctrl Pts',(-202.538262705644,63.546434789606,17.));
#17620=CARTESIAN_POINT('Ctrl Pts',(-202.546434285539,63.5295449770387,17.));
#17621=CARTESIAN_POINT('Ctrl Pts',(-202.554766777349,63.5127432414087,17.));
#17622=CARTESIAN_POINT('Ctrl Pts',(-202.597561732177,63.426450985303,17.));
#17623=CARTESIAN_POINT('Ctrl Pts',(-202.644651926136,63.3423600645501,17.));
#17624=CARTESIAN_POINT('Ctrl Pts',(-202.695691913412,63.2607170650344,17.));
#17625=CARTESIAN_POINT('Ctrl Pts',(-202.747749229102,63.17744675823,17.));
#17626=CARTESIAN_POINT('Ctrl Pts',(-202.803915679762,63.0967221624598,17.));
#17627=CARTESIAN_POINT('Ctrl Pts',(-202.863879846291,63.0188121011017,17.));
#17628=CARTESIAN_POINT('Ctrl Pts',(-202.92434189817,62.9402551487678,17.));
#17629=CARTESIAN_POINT('Ctrl Pts',(-202.98866545666,62.8645588312244,17.));
#17630=CARTESIAN_POINT('Ctrl Pts',(-203.056580646588,62.7920181029229,17.));
#17631=CARTESIAN_POINT('Ctrl Pts',(-203.094626893211,62.7513806189939,17.));
#17632=CARTESIAN_POINT('Ctrl Pts',(-203.133801134145,62.71173385957,17.));
#17633=CARTESIAN_POINT('Ctrl Pts',(-203.174061757578,62.673133821284,17.));
#17634=CARTESIAN_POINT('Ctrl Pts',(-203.185603246106,62.6620683716942,17.));
#17635=CARTESIAN_POINT('Ctrl Pts',(-203.197234036914,62.6510889631318,17.));
#17636=CARTESIAN_POINT('Ctrl Pts',(-203.208953206155,62.6401969707666,17.));
#17637=CARTESIAN_POINT('Ctrl Pts',(-203.219358434025,62.6305261775393,17.));
#17638=CARTESIAN_POINT('Ctrl Pts',(-203.229830124301,62.6209273315836,17.));
#17639=CARTESIAN_POINT('Ctrl Pts',(-203.240361443976,62.6114066232139,17.));
#17640=CARTESIAN_POINT('Ctrl Pts',(-203.316072000031,62.5429614380971,17.));
#17641=CARTESIAN_POINT('Ctrl Pts',(-203.394951774449,62.4784678301501,17.));
#17642=CARTESIAN_POINT('Ctrl Pts',(-203.476670244702,62.4182049299063,17.));
#17643=CARTESIAN_POINT('Ctrl Pts',(-203.558481705369,62.3578734543199,17.));
#17644=CARTESIAN_POINT('Ctrl Pts',(-203.643138907573,62.3017814875231,17.));
#17645=CARTESIAN_POINT('Ctrl Pts',(-203.730355413283,62.2502350560919,17.));
#17646=CARTESIAN_POINT('Ctrl Pts',(-203.815753129695,62.1997635599272,17.));
#17647=CARTESIAN_POINT('Ctrl Pts',(-203.903605194206,62.1536493286983,17.));
#17648=CARTESIAN_POINT('Ctrl Pts',(-203.99367653385,62.1122153753288,17.));
#17649=CARTESIAN_POINT('Ctrl Pts',(-204.044060613228,62.0890380627258,17.));
#17650=CARTESIAN_POINT('Ctrl Pts',(-204.095139669776,62.0673259342666,17.));
#17651=CARTESIAN_POINT('Ctrl Pts',(-204.146876157629,62.0471417471569,17.));
#17652=CARTESIAN_POINT('Ctrl Pts',(-204.165972597182,62.0396915678916,17.));
#17653=CARTESIAN_POINT('Ctrl Pts',(-204.185158628751,62.0324496078491,17.));
#17654=CARTESIAN_POINT('Ctrl Pts',(-204.204431285565,62.0254151804089,17.));
#17655=CARTESIAN_POINT('Ctrl Pts',(-205.793799282533,62.0307770462544,17.));
#17656=CARTESIAN_POINT('Ctrl Pts',(-205.888627163302,62.0654655086331,17.));
#17657=CARTESIAN_POINT('Ctrl Pts',(-205.98140929384,62.1051486930793,17.));
#17658=CARTESIAN_POINT('Ctrl Pts',(-206.071905809173,62.1495050655195,17.));
#17659=CARTESIAN_POINT('Ctrl Pts',(-206.163687726546,62.1944914707457,17.));
#17660=CARTESIAN_POINT('Ctrl Pts',(-206.253119305857,62.2442854648945,17.));
#17661=CARTESIAN_POINT('Ctrl Pts',(-206.339916279455,62.2985923241862,17.));
#17662=CARTESIAN_POINT('Ctrl Pts',(-206.364296640601,62.3138465523854,17.));
#17663=CARTESIAN_POINT('Ctrl Pts',(-206.388468896561,62.329457048441,17.));
#17664=CARTESIAN_POINT('Ctrl Pts',(-206.412426161583,62.3454177286137,17.));
#17665=CARTESIAN_POINT('Ctrl Pts',(-206.431863584532,62.3583672239246,17.));
#17666=CARTESIAN_POINT('Ctrl Pts',(-206.451161692209,62.3715489324215,17.));
#17667=CARTESIAN_POINT('Ctrl Pts',(-206.470297259089,62.3849456542333,17.));
#17668=CARTESIAN_POINT('Ctrl Pts',(-206.553008850231,62.4428516563967,17.));
#17669=CARTESIAN_POINT('Ctrl Pts',(-206.632764575627,62.5048222618196,17.));
#17670=CARTESIAN_POINT('Ctrl Pts',(-206.709299005451,62.5705587218441,17.));
#17671=CARTESIAN_POINT('Ctrl Pts',(-206.768827177178,62.621688276087,17.));
#17672=CARTESIAN_POINT('Ctrl Pts',(-206.826405951603,62.6750969629653,17.));
#17673=CARTESIAN_POINT('Ctrl Pts',(-206.88189230934,62.7306563357683,17.));
#17674=CARTESIAN_POINT('Ctrl Pts',(-206.912069704626,62.760873441797,17.));
#17675=CARTESIAN_POINT('Ctrl Pts',(-206.941627879906,62.7917268692334,17.));
#17676=CARTESIAN_POINT('Ctrl Pts',(-206.970541572236,62.8231968742563,17.));
#17677=CARTESIAN_POINT('Ctrl Pts',(-206.982346396854,62.8360453851206,17.));
#17678=CARTESIAN_POINT('Ctrl Pts',(-206.994038687849,62.8489912085626,17.));
#17679=CARTESIAN_POINT('Ctrl Pts',(-207.005612070685,62.8620271047964,17.));
#17680=CARTESIAN_POINT('Ctrl Pts',(-207.071011765377,62.9356912741935,17.));
#17681=CARTESIAN_POINT('Ctrl Pts',(-207.132669287851,63.0122850945349,17.));
#17682=CARTESIAN_POINT('Ctrl Pts',(-207.190339507946,63.0915302946758,17.));
#17683=CARTESIAN_POINT('Ctrl Pts',(-207.247552291736,63.1701469272205,17.));
#17684=CARTESIAN_POINT('Ctrl Pts',(-207.300841218128,63.2513738284823,17.));
#17685=CARTESIAN_POINT('Ctrl Pts',(-207.349920642778,63.3349611348081,17.));
#17686=CARTESIAN_POINT('Ctrl Pts',(-207.397481392412,63.4159619814392,17.));
#17687=CARTESIAN_POINT('Ctrl Pts',(-207.441089305762,63.4991801155586,17.));
#17688=CARTESIAN_POINT('Ctrl Pts',(-207.480436533273,63.5843978591788,17.));
#17689=CARTESIAN_POINT('Ctrl Pts',(-207.501052452161,63.629047563909,17.));
#17690=CARTESIAN_POINT('Ctrl Pts',(-207.520497896918,63.6742463055229,17.));
#17691=CARTESIAN_POINT('Ctrl Pts',(-207.538722823233,63.7199629468458,17.));
#17692=CARTESIAN_POINT('Ctrl Pts',(-207.545019377446,63.7357576505121,17.));
#17693=CARTESIAN_POINT('Ctrl Pts',(-207.551170208915,63.7516141714125,17.));
#17694=CARTESIAN_POINT('Ctrl Pts',(-207.557173136494,63.7675312180113,17.));
#17695=CARTESIAN_POINT('Ctrl Pts',(-207.562735096129,63.7822790172345,17.));
#17696=CARTESIAN_POINT('Ctrl Pts',(-207.568167313965,63.7970715617822,17.));
#17697=CARTESIAN_POINT('Ctrl Pts',(-207.573465961202,63.8119004887879,17.));
#17698=CARTESIAN_POINT('Ctrl Pts',(-207.604700101148,63.8993131359471,17.));
#17699=CARTESIAN_POINT('Ctrl Pts',(-207.631326724125,63.9880676646163,17.));
#17700=CARTESIAN_POINT('Ctrl Pts',(-207.653093596572,64.0779404437609,17.));
#17701=CARTESIAN_POINT('Ctrl Pts',(-207.658254733772,64.0992501539593,17.));
#17702=CARTESIAN_POINT('Ctrl Pts',(-207.663142425011,64.1206227749284,17.));
#17703=CARTESIAN_POINT('Ctrl Pts',(-207.667752876821,64.1420553867836,17.));
#17704=CARTESIAN_POINT('Ctrl Pts',(-207.687563068899,64.2341470461388,17.));
#17705=CARTESIAN_POINT('Ctrl Pts',(-207.702258853542,64.3273466761675,17.));
#17706=CARTESIAN_POINT('Ctrl Pts',(-207.711951692842,64.4212621179871,17.));
#17707=CARTESIAN_POINT('Ctrl Pts',(-207.722120103753,64.5197854478193,17.));
#17708=CARTESIAN_POINT('Ctrl Pts',(-207.726782615872,64.6190978352621,17.));
#17709=CARTESIAN_POINT('Ctrl Pts',(-207.726009639275,64.718730548459,17.));
#17710=CARTESIAN_POINT('Ctrl Pts',(-207.725769558652,64.7496757076122,17.));
#17711=CARTESIAN_POINT('Ctrl Pts',(-207.725004722666,64.7806515775433,17.));
#17712=CARTESIAN_POINT('Ctrl Pts',(-207.723716174804,64.8116435095492,17.));
#17713=CARTESIAN_POINT('Ctrl Pts',(-207.723127503835,64.8258021226421,17.));
#17714=CARTESIAN_POINT('Ctrl Pts',(-207.722429444061,64.8399641697794,17.));
#17715=CARTESIAN_POINT('Ctrl Pts',(-207.721623107401,64.8541137317494,17.));
#17716=CARTESIAN_POINT('Ctrl Pts',(-207.716331548034,64.9469697940972,17.));
#17717=CARTESIAN_POINT('Ctrl Pts',(-207.706375553367,65.0394451487277,17.));
#17718=CARTESIAN_POINT('Ctrl Pts',(-207.691882946519,65.131168594172,17.));
#17719=CARTESIAN_POINT('Ctrl Pts',(-207.677420973782,65.2226981568877,17.));
#17720=CARTESIAN_POINT('Ctrl Pts',(-207.658441130303,65.3134799320582,17.));
#17721=CARTESIAN_POINT('Ctrl Pts',(-207.635021707819,65.4031281056214,17.));
#17722=CARTESIAN_POINT('Ctrl Pts',(-207.611997363202,65.4912639443185,17.));
#17723=CARTESIAN_POINT('Ctrl Pts',(-207.584681489474,65.578304892392,17.));
#17724=CARTESIAN_POINT('Ctrl Pts',(-207.553108104886,65.6638552077799,17.));
#17725=CARTESIAN_POINT('Ctrl Pts',(-207.536805169438,65.708029162759,17.));
#17726=CARTESIAN_POINT('Ctrl Pts',(-207.519366485957,65.7518051379706,17.));
#17727=CARTESIAN_POINT('Ctrl Pts',(-207.500793026226,65.7951245042335,17.));
#17728=CARTESIAN_POINT('Ctrl Pts',(-207.49498264897,65.8086761991856,17.));
#17729=CARTESIAN_POINT('Ctrl Pts',(-207.489060429026,65.822184902516,17.));
#17730=CARTESIAN_POINT('Ctrl Pts',(-207.483028782271,65.8356433357431,17.));
#17731=CARTESIAN_POINT('Ctrl Pts',(-207.446484708349,65.9171842479814,17.));
#17732=CARTESIAN_POINT('Ctrl Pts',(-207.406050922741,65.9966090453918,17.));
#17733=CARTESIAN_POINT('Ctrl Pts',(-207.361807140979,66.0735724370544,17.));
#17734=CARTESIAN_POINT('Ctrl Pts',(-207.318274246064,66.149299219623,17.));
#17735=CARTESIAN_POINT('Ctrl Pts',(-207.271052339791,66.2226437477733,17.));
#17736=CARTESIAN_POINT('Ctrl Pts',(-207.220180215582,66.2932441543424,17.));
#17737=CARTESIAN_POINT('Ctrl Pts',(-207.170937073537,66.3615838571394,17.));
#17738=CARTESIAN_POINT('Ctrl Pts',(-207.118273276478,66.4273528076824,17.));
#17739=CARTESIAN_POINT('Ctrl Pts',(-207.06219578552,66.4901836495188,17.));
#17740=CARTESIAN_POINT('Ctrl Pts',(-207.027350691367,66.5292251002338,17.));
#17741=CARTESIAN_POINT('Ctrl Pts',(-206.991187020073,66.5671313315531,17.));
#17742=CARTESIAN_POINT('Ctrl Pts',(-206.953701799746,66.6038050912543,17.));
#17743=CARTESIAN_POINT('Ctrl Pts',(-206.941652995692,66.6155930690407,17.));
#17744=CARTESIAN_POINT('Ctrl Pts',(-206.929467627116,66.6272536523146,17.));
#17745=CARTESIAN_POINT('Ctrl Pts',(-206.917148172614,66.6387856228502,17.));
#17746=CARTESIAN_POINT('Origin',(-205.,65.,-2.20842344717744));
#17747=CARTESIAN_POINT('Ctrl Pts',(-201.923731627295,65.0022750736124,0.291576552822547));
#17748=CARTESIAN_POINT('Ctrl Pts',(-201.922496052185,65.1502516884003,0.299259877064296));
#17749=CARTESIAN_POINT('Ctrl Pts',(-201.999549699837,66.317125995226,0.359912640907481));
#17750=CARTESIAN_POINT('Ctrl Pts',(-203.493276988919,68.3070967035895,0.473534844352101));
#17751=CARTESIAN_POINT('Ctrl Pts',(-206.96385777596,68.0574739600344,0.632443163156408));
#17752=CARTESIAN_POINT('Ctrl Pts',(-208.633920120295,65.0051924190987,0.791351481960715));
#17753=CARTESIAN_POINT('Ctrl Pts',(-206.972481828636,61.9479566315291,0.95025980076502));
#17754=CARTESIAN_POINT('Ctrl Pts',(-203.502676407862,61.6888942785303,1.10916811956933));
#17755=CARTESIAN_POINT('Ctrl Pts',(-202.001256849451,63.6767448554868,1.22294037025517));
#17756=CARTESIAN_POINT('Ctrl Pts',(-201.922527685932,64.8467465056595,1.28374318133958));
#17757=CARTESIAN_POINT('Ctrl Pts',(-201.923803965215,64.9976529174956,1.29157655282255));
#17758=CARTESIAN_POINT('Ctrl Pts',(-201.929611540575,64.9968423971894,0.208423447177456));
#17759=CARTESIAN_POINT('Ctrl Pts',(-201.934956993548,65.702126874876,0.244887843987842));
#17760=CARTESIAN_POINT('Ctrl Pts',(-202.52503086706,67.4423464487146,0.334321680399663));
#17761=CARTESIAN_POINT('Ctrl Pts',(-205.417645976078,68.6092463233164,0.47672495641292));
#17762=CARTESIAN_POINT('Ctrl Pts',(-208.260115679803,66.6049913509854,0.635633275217227));
#17763=CARTESIAN_POINT('Ctrl Pts',(-208.114970174343,63.128085617879,0.794541594021532));
#17764=CARTESIAN_POINT('Ctrl Pts',(-205.113461133577,61.3679192540746,0.95344991282584));
#17765=CARTESIAN_POINT('Ctrl Pts',(-202.417561343649,62.7304356237314,1.09141053054448));
#17766=CARTESIAN_POINT('Ctrl Pts',(-201.93359519178,64.3813018489966,1.17640170866169));
#17767=CARTESIAN_POINT('Ctrl Pts',(-201.930557054308,65.0016530359719,1.20842344717746));
#17768=CARTESIAN_POINT('Ctrl Pts',(-206.913465996665,66.6359872033749,0.));
#17769=CARTESIAN_POINT('Ctrl Pts',(-207.457950030113,65.9991535645904,0.0529694396014356));
#17770=CARTESIAN_POINT('Ctrl Pts',(-207.850661636903,64.1491413375017,0.158908318804307));
#17771=CARTESIAN_POINT('Ctrl Pts',(-205.826538235528,62.1387920084224,0.317816637608613));
#17772=CARTESIAN_POINT('Ctrl Pts',(-203.043492655661,62.757459158079,0.47672495641292));
#17773=CARTESIAN_POINT('Ctrl Pts',(-202.054683559188,65.4291982286823,0.635633275217226));
#17774=CARTESIAN_POINT('Ctrl Pts',(-203.76584506901,67.7088387672967,0.794541594021534));
#17775=CARTESIAN_POINT('Ctrl Pts',(-206.608593444275,67.504373090739,0.953449912825839));
#17776=CARTESIAN_POINT('Ctrl Pts',(-207.976539418527,65.0042531039795,1.11235823163015));
#17777=CARTESIAN_POINT('Ctrl Pts',(-206.615657395019,62.500075100008,1.27126655043445));
#17778=CARTESIAN_POINT('Ctrl Pts',(-203.773544121293,62.2878774511794,1.43017486923876));
#17779=CARTESIAN_POINT('Ctrl Pts',(-202.055838985475,64.5620859668133,1.58908318804307));
#17780=CARTESIAN_POINT('Ctrl Pts',(-203.037304314461,67.237787377709,1.74799150684737));
#17781=CARTESIAN_POINT('Ctrl Pts',(-205.818148785739,67.8619014891644,1.90689982565168));
#17782=CARTESIAN_POINT('Ctrl Pts',(-207.848922781157,65.8622605977419,2.06580814445599));
#17783=CARTESIAN_POINT('Ctrl Pts',(-207.267836607737,63.0721067410292,2.22471646326029));
#17784=CARTESIAN_POINT('Ctrl Pts',(-204.607622987557,62.0494248900596,2.3836247820646));
#17785=CARTESIAN_POINT('Ctrl Pts',(-202.307136320099,63.7317968295565,2.54253310086891));
#17786=CARTESIAN_POINT('Ctrl Pts',(-202.475436931506,66.57684350044,2.70144141967321));
#17787=CARTESIAN_POINT('Ctrl Pts',(-204.958228769587,67.9762575579951,2.86034973847752));
#17788=CARTESIAN_POINT('Ctrl Pts',(-207.479315994157,66.6470720078308,3.01925805728183));
#17789=CARTESIAN_POINT('Ctrl Pts',(-207.727394031276,63.8078692224566,3.17816637608614));
#17790=CARTESIAN_POINT('Ctrl Pts',(-205.475027701519,62.0615986230515,3.33707469489044));
#17791=CARTESIAN_POINT('Ctrl Pts',(-202.787161285521,63.0092215576596,3.49598301369475));
#17792=CARTESIAN_POINT('Ctrl Pts',(-202.128000669921,65.7819679208284,3.65489133249905));
#17793=CARTESIAN_POINT('Ctrl Pts',(-204.101856940684,67.8378148325493,3.81379965130336));
#17794=CARTESIAN_POINT('Ctrl Pts',(-206.899120729728,67.2919848242,3.97270797010767));
#17795=CARTESIAN_POINT('Ctrl Pts',(-207.955291859906,64.6448887457045,4.13161628891197));
#17796=CARTESIAN_POINT('Ctrl Pts',(-206.302084443574,62.323354696317,4.29052460771628));
#17797=CARTESIAN_POINT('Ctrl Pts',(-203.455140562519,62.4557391449499,4.44943292652058));
#17798=CARTESIAN_POINT('Ctrl Pts',(-202.024506547164,64.9206735088564,4.60834124532489));
#17799=CARTESIAN_POINT('Ctrl Pts',(-203.321771672898,67.4583335132076,4.7672495641292));
#17800=CARTESIAN_POINT('Ctrl Pts',(-206.157617771706,67.7422208289451,4.92615788293351));
#17801=CARTESIAN_POINT('Ctrl Pts',(-207.93217283587,65.5120707379364,5.08506620173782));
#17802=CARTESIAN_POINT('Ctrl Pts',(-207.018544616397,62.8124599176985,5.24397452054212));
#17803=CARTESIAN_POINT('Ctrl Pts',(-204.254337253468,62.1183613952304,5.40288283934643));
#17804=CARTESIAN_POINT('Ctrl Pts',(-202.173745162441,64.0661169381366,5.56179115815074));
#17805=CARTESIAN_POINT('Ctrl Pts',(-202.684231918022,66.870046034341,5.72069947695504));
#17806=CARTESIAN_POINT('Ctrl Pts',(-205.3177889683,67.9595378273796,5.87960779575935));
#17807=CARTESIAN_POINT('Ctrl Pts',(-207.660000644302,66.3357584184189,6.03851611456366));
#17808=CARTESIAN_POINT('Ctrl Pts',(-207.563553459886,63.4873706209475,6.19742443336795));
#17809=CARTESIAN_POINT('Ctrl Pts',(-205.116869115753,62.0257445318455,6.35633275217228));
#17810=CARTESIAN_POINT('Ctrl Pts',(-202.56304047252,63.2908826133093,6.51524107097657));
#17811=CARTESIAN_POINT('Ctrl Pts',(-202.243389086688,66.1229204124393,6.67414938978089));
#17812=CARTESIAN_POINT('Ctrl Pts',(-204.45096777611,67.9254773280944,6.83305770858519));
#17813=CARTESIAN_POINT('Ctrl Pts',(-207.161893071975,67.0459893268077,6.99196602738949));
#17814=CARTESIAN_POINT('Ctrl Pts',(-207.890818962485,64.2907611783034,7.1508743461938));
#17815=CARTESIAN_POINT('Ctrl Pts',(-205.969474338275,62.185755254515,7.30978266499811));
#17816=CARTESIAN_POINT('Ctrl Pts',(-203.159326476349,62.6608174591554,7.46869098380242));
#17817=CARTESIAN_POINT('Ctrl Pts',(-202.036687528078,65.2804160726826,7.62759930260672));
#17818=CARTESIAN_POINT('Ctrl Pts',(-203.630780333736,67.6429323649268,7.78650762141104));
#17819=CARTESIAN_POINT('Ctrl Pts',(-206.480158425938,67.5824378045147,7.94541594021533));
#17820=CARTESIAN_POINT('Ctrl Pts',(-207.972543816666,65.154393128297,8.10432425901965));
#17821=CARTESIAN_POINT('Ctrl Pts',(-206.739734259782,62.5848025576766,8.26323257782394));
#17822=CARTESIAN_POINT('Ctrl Pts',(-203.91195577818,62.2294380080158,8.42214089662826));
#17823=CARTESIAN_POINT('Ctrl Pts',(-202.081684078297,64.4140937266076,8.58104921543256));
#17824=CARTESIAN_POINT('Ctrl Pts',(-202.926891798018,67.1359017680923,8.73995753423687));
#17825=CARTESIAN_POINT('Ctrl Pts',(-205.672701946614,67.8995389411223,8.89886585304117));
#17826=CARTESIAN_POINT('Ctrl Pts',(-207.801786469205,66.0049112204788,9.05777417184548));
#17827=CARTESIAN_POINT('Ctrl Pts',(-207.362224471816,63.1889921245852,9.21668249064979));
#17828=CARTESIAN_POINT('Ctrl Pts',(-204.757001480761,62.0333848076113,9.37559080945409));
#17829=CARTESIAN_POINT('Ctrl Pts',(-202.3745568162,63.5975371417748,9.53449912825841));
#17830=CARTESIAN_POINT('Ctrl Pts',(-202.399089118511,66.4474517493217,9.6934074470627));
#17831=CARTESIAN_POINT('Ctrl Pts',(-204.808107447128,67.9703587709594,9.85231576586701));
#17832=CARTESIAN_POINT('Ctrl Pts',(-207.393050723475,66.7700740704675,10.0112240846713));
#17833=CARTESIAN_POINT('Ctrl Pts',(-207.784071843173,63.9470052459228,10.1701324034756));
#17834=CARTESIAN_POINT('Ctrl Pts',(-205.622687014046,62.0893102428115,10.3290407222799));
#17835=CARTESIAN_POINT('Ctrl Pts',(-202.890429690085,62.900103076913,10.4879490410842));
#17836=CARTESIAN_POINT('Ctrl Pts',(-202.092202848023,65.6360579399868,10.6468573598885));
#17837=CARTESIAN_POINT('Ctrl Pts',(-203.959811935046,67.7888819927689,10.8057656786929));
#17838=CARTESIAN_POINT('Ctrl Pts',(-206.781053814051,67.3848902053379,10.9646739974972));
#17839=CARTESIAN_POINT('Ctrl Pts',(-207.969445462805,64.7944577330778,11.1235823163015));
#17840=CARTESIAN_POINT('Ctrl Pts',(-206.435482700137,62.3924641138286,11.2824906351058));
#17841=CARTESIAN_POINT('Ctrl Pts',(-203.585485442077,62.3810302511319,11.4413989539101));
#17842=CARTESIAN_POINT('Ctrl Pts',(-202.032299320984,64.770638582514,11.6003072727144));
#17843=CARTESIAN_POINT('Ctrl Pts',(-203.199868013036,67.3705228979221,11.7592155915187));
#17844=CARTESIAN_POINT('Ctrl Pts',(-206.017777591034,67.7971383153597,11.918123910323));
#17845=CARTESIAN_POINT('Ctrl Pts',(-207.902600049061,65.6593685883118,12.0770322291273));
#17846=CARTESIAN_POINT('Ctrl Pts',(-207.12635122387,62.9170971091267,12.2359405479316));
#17847=CARTESIAN_POINT('Ctrl Pts',(-204.400687362422,62.0844077201178,12.3948488667359));
#17848=CARTESIAN_POINT('Ctrl Pts',(-202.224466628715,63.924700746336,12.5537571855402));
#17849=CARTESIAN_POINT('Ctrl Pts',(-202.592823868233,66.7508161099091,12.7126655043445));
#17850=CARTESIAN_POINT('Ctrl Pts',(-205.168053280859,67.9718028324414,12.8715738231488));
#17851=CARTESIAN_POINT('Ctrl Pts',(-207.589213323861,66.4682739333878,13.0304821419531));
#17852=CARTESIAN_POINT('Ctrl Pts',(-207.63661153071,63.6186479028593,13.1893904607575));
#17853=CARTESIAN_POINT('Ctrl Pts',(-205.26679375494,62.0354300357772,13.3482987795618));
#17854=CARTESIAN_POINT('Ctrl Pts',(-202.652382446799,63.1700967777672,13.5072070983661));
#17855=CARTESIAN_POINT('Ctrl Pts',(-202.190240672061,65.9823983409187,13.6661154171704));
#17856=CARTESIAN_POINT('Ctrl Pts',(-204.304054846181,67.8940480862733,13.8250237359747));
#17857=CARTESIAN_POINT('Ctrl Pts',(-207.055903756617,67.1524668900571,13.983932054779));
#17858=CARTESIAN_POINT('Ctrl Pts',(-207.922923086071,64.437528111351,14.1428403735833));
#17859=CARTESIAN_POINT('Ctrl Pts',(-206.110239189501,62.2382572639803,14.3017486923876));
#17860=CARTESIAN_POINT('Ctrl Pts',(-203.279700432717,62.5709213092164,14.4606570111919));
#17861=CARTESIAN_POINT('Ctrl Pts',(-202.026313051011,65.1305375083974,14.6195653299962));
#17862=CARTESIAN_POINT('Ctrl Pts',(-203.499168711792,67.5704784621524,14.7784736488005));
#17863=CARTESIAN_POINT('Ctrl Pts',(-206.347969550324,67.6538333200658,14.9373819676048));
#17864=CARTESIAN_POINT('Ctrl Pts',(-207.96096732682,65.3041838044336,15.0962902864091));
#17865=CARTESIAN_POINT('Ctrl Pts',(-206.859382619904,62.6756612501156,15.2551986052134));
#17866=CARTESIAN_POINT('Ctrl Pts',(-204.053138216533,62.1780679787958,15.4141069240178));
#17867=CARTESIAN_POINT('Ctrl Pts',(-202.114963009909,64.2675873651587,15.5730152428221));
#17868=CARTESIAN_POINT('Ctrl Pts',(-202.821763859197,67.0285808080553,15.7319235616264));
#17869=CARTESIAN_POINT('Ctrl Pts',(-205.525534104406,67.9297809896548,15.8908318804307));
#17870=CARTESIAN_POINT('Ctrl Pts',(-207.747527632094,66.1450175695412,16.049740199235));
#17871=CARTESIAN_POINT('Ctrl Pts',(-207.450562796655,63.3104595362684,16.2086485180393));
#17872=CARTESIAN_POINT('Ctrl Pts',(-204.907064123563,62.0249671649789,16.3675568368436));
#17873=CARTESIAN_POINT('Ctrl Pts',(-202.448531805715,63.4667172751089,16.5264651556479));
#17874=CARTESIAN_POINT('Ctrl Pts',(-202.329643294205,66.314646385853,16.6853734744522));
#17875=CARTESIAN_POINT('Ctrl Pts',(-204.657906700394,67.9563292425747,16.8442817932565));
#17876=CARTESIAN_POINT('Ctrl Pts',(-207.301858734717,66.8897415144046,17.0031901120608));
#17877=CARTESIAN_POINT('Ctrl Pts',(-207.831197468937,64.0864612085167,17.1620984308651));
#17878=CARTESIAN_POINT('Ctrl Pts',(-206.459639356019,62.7843106836637,17.268037310068));
#17879=CARTESIAN_POINT('Ctrl Pts',(-205.650199997975,62.567913197965,17.3210067496694));
#17880=CARTESIAN_POINT('Ctrl Pts',(-207.054331550342,66.7564253212268,-0.107002249889811));
#17881=CARTESIAN_POINT('Ctrl Pts',(-207.63889941333,66.0727092589846,-0.0540328102883751));
#17882=CARTESIAN_POINT('Ctrl Pts',(-208.060521666048,64.0865028182897,0.0519060689144961));
#17883=CARTESIAN_POINT('Ctrl Pts',(-205.88738633337,61.9281555776621,0.210814387718803));
#17884=CARTESIAN_POINT('Ctrl Pts',(-202.899458483737,62.5923677700475,0.36972270652311));
#17885=CARTESIAN_POINT('Ctrl Pts',(-201.837855231999,65.4607949470069,0.528631025327416));
#17886=CARTESIAN_POINT('Ctrl Pts',(-203.674989042313,67.9082580793944,0.687539344131723));
#17887=CARTESIAN_POINT('Ctrl Pts',(-206.72701488817,67.6887400471708,0.846447662936029));
#17888=CARTESIAN_POINT('Ctrl Pts',(-208.195666319116,65.0045662090192,1.00535598174034));
#17889=CARTESIAN_POINT('Ctrl Pts',(-206.734598872892,62.316035610515,1.16426430054464));
#17890=CARTESIAN_POINT('Ctrl Pts',(-203.683254883482,62.0882163936298,1.32317261934895));
#17891=CARTESIAN_POINT('Ctrl Pts',(-201.839095718467,64.5298476083291,1.48208093815326));
#17892=CARTESIAN_POINT('Ctrl Pts',(-202.89281456919,67.4025288251776,1.64098925695756));
#17893=CARTESIAN_POINT('Ctrl Pts',(-205.878379269006,68.0725889738351,1.79989757576187));
#17894=CARTESIAN_POINT('Ctrl Pts',(-208.058654799208,65.9257385047058,1.95880589456618));
#17895=CARTESIAN_POINT('Ctrl Pts',(-207.43479021964,62.9301790810506,2.11771421337048));
#17896=CARTESIAN_POINT('Ctrl Pts',(-204.578736973798,61.8322094301289,2.27662253217479));
#17897=CARTESIAN_POINT('Ctrl Pts',(-202.108893062102,63.6384342393193,2.4355308509791));
#17898=CARTESIAN_POINT('Ctrl Pts',(-202.289583629145,66.6929275767385,2.5944391697834));
#17899=CARTESIAN_POINT('Ctrl Pts',(-204.955153654843,68.1953637085738,2.75334748858771));
#17900=CARTESIAN_POINT('Ctrl Pts',(-207.66183829707,66.7683261668979,2.91225580739201));
#17901=CARTESIAN_POINT('Ctrl Pts',(-207.928179344933,63.7201069301938,3.07116412619632));
#17902=CARTESIAN_POINT('Ctrl Pts',(-205.509998294309,61.8452793690848,3.23007244500063));
#17903=CARTESIAN_POINT('Ctrl Pts',(-202.624256508924,62.8626644157938,3.38898076380494));
#17904=CARTESIAN_POINT('Ctrl Pts',(-201.916569802324,65.8395348409185,3.54788908260924));
#17905=CARTESIAN_POINT('Ctrl Pts',(-204.035737438403,68.0467291055579,3.70679740141355));
#17906=CARTESIAN_POINT('Ctrl Pts',(-207.038930213439,67.460716179679,3.86570572021786));
#17907=CARTESIAN_POINT('Ctrl Pts',(-208.17285455757,64.6187461627998,4.02461403902216));
#17908=CARTESIAN_POINT('Ctrl Pts',(-206.397941305624,62.1263054028582,4.18352235782647));
#17909=CARTESIAN_POINT('Ctrl Pts',(-203.3414110892,62.2684357307946,4.34243067663078));
#17910=CARTESIAN_POINT('Ctrl Pts',(-201.805456648484,64.9148336506537,4.50133899543508));
#17911=CARTESIAN_POINT('Ctrl Pts',(-203.198223847691,67.6393111276853,4.66024731423939));
#17912=CARTESIAN_POINT('Ctrl Pts',(-206.242839285253,67.9440976619002,4.8191556330437));
#17913=CARTESIAN_POINT('Ctrl Pts',(-208.148033557054,65.5497683652509,4.978063951848));
#17914=CARTESIAN_POINT('Ctrl Pts',(-207.167145848667,62.6514175759892,5.13697227065231));
#17915=CARTESIAN_POINT('Ctrl Pts',(-204.199443047964,61.9062209034394,5.29588058945662));
#17916=CARTESIAN_POINT('Ctrl Pts',(-201.965681913227,63.9973663280875,5.45478890826092));
#17917=CARTESIAN_POINT('Ctrl Pts',(-202.513749686499,67.0077150969155,5.61369722706523));
#17918=CARTESIAN_POINT('Ctrl Pts',(-205.341183958882,68.1774131047081,5.77260554586954));
#17919=CARTESIAN_POINT('Ctrl Pts',(-207.855824591105,66.4340942913934,5.93151386467385));
#17920=CARTESIAN_POINT('Ctrl Pts',(-207.752277157164,63.3760138603049,6.09042218347815));
#17921=CARTESIAN_POINT('Ctrl Pts',(-205.125472787168,61.8067857711313,6.24933050228246));
#17922=CARTESIAN_POINT('Ctrl Pts',(-202.38363636828,63.1650607970895,6.40823882108677));
#17923=CARTESIAN_POINT('Ctrl Pts',(-202.040452884397,66.2055875755397,6.56714713989107));
#17924=CARTESIAN_POINT('Ctrl Pts',(-204.410549117854,68.1408451393384,6.72605545869538));
#17925=CARTESIAN_POINT('Ctrl Pts',(-207.321047331891,67.1966109839683,6.88496377749969));
#17926=CARTESIAN_POINT('Ctrl Pts',(-208.103635293917,64.2385484295628,7.04387209630399));
#17927=CARTESIAN_POINT('Ctrl Pts',(-206.04084510717,61.9785761643475,7.2027804151083));
#17928=CARTESIAN_POINT('Ctrl Pts',(-203.02381975948,62.4886115018288,7.36168873391261));
#17929=CARTESIAN_POINT('Ctrl Pts',(-201.818534368941,65.3010597451634,7.52059705271691));
#17930=CARTESIAN_POINT('Ctrl Pts',(-203.529981110373,67.8374997790149,7.67950537152123));
#17931=CARTESIAN_POINT('Ctrl Pts',(-206.589124739718,67.7725517296137,7.83841369032552));
#17932=CARTESIAN_POINT('Ctrl Pts',(-208.191376569008,65.1657592427404,7.99732200912984));
#17933=CARTESIAN_POINT('Ctrl Pts',(-206.867810029188,62.4070005347793,8.15623032793413));
#17934=CARTESIAN_POINT('Ctrl Pts',(-203.831856130734,62.0254747551137,8.31513864673844));
#17935=CARTESIAN_POINT('Ctrl Pts',(-201.866843475521,64.3709604743062,8.47404696554275));
#17936=CARTESIAN_POINT('Ctrl Pts',(-202.774273703308,67.2931426000101,8.63295528434706));
#17937=CARTESIAN_POINT('Ctrl Pts',(-205.722224923419,68.1129972200054,8.79186360315136));
#17938=CARTESIAN_POINT('Ctrl Pts',(-208.008048405898,66.0788907820261,8.95077192195567));
#17939=CARTESIAN_POINT('Ctrl Pts',(-207.536126730185,63.0556693336245,9.10968024075997));
#17940=CARTESIAN_POINT('Ctrl Pts',(-204.739112414002,61.8149885087741,9.26858855956429));
#17941=CARTESIAN_POINT('Ctrl Pts',(-202.181276920776,63.4942906208646,9.42749687836859));
#17942=CARTESIAN_POINT('Ctrl Pts',(-202.207615242297,66.5540102627441,9.5864051971729));
#17943=CARTESIAN_POINT('Ctrl Pts',(-204.793980699773,68.1890306645911,9.7453135159772));
#17944=CARTESIAN_POINT('Ctrl Pts',(-207.569222349063,66.9003833962775,9.90422183478151));
#17945=CARTESIAN_POINT('Ctrl Pts',(-207.989029664398,63.8694858704489,10.0631301535858));
#17946=CARTESIAN_POINT('Ctrl Pts',(-205.668527991181,61.8750310630701,10.2220384723901));
#17947=CARTESIAN_POINT('Ctrl Pts',(-202.735127327647,62.745512849937,10.3809467911944));
#17948=CARTESIAN_POINT('Ctrl Pts',(-201.878136616114,65.6828832580448,10.5398551099987));
#17949=CARTESIAN_POINT('Ctrl Pts',(-203.883235362505,67.9941939276222,10.698763428803));
#17950=CARTESIAN_POINT('Ctrl Pts',(-206.912171446705,67.560461069842,10.8576717476073));
#17951=CARTESIAN_POINT('Ctrl Pts',(-208.18805012051,64.7793261209747,11.0165800664117));
#17952=CARTESIAN_POINT('Ctrl Pts',(-206.541160076009,62.2005025179714,11.175488385216));
#17953=CARTESIAN_POINT('Ctrl Pts',(-203.48135169905,62.1882269170874,11.3343967040203));
#17954=CARTESIAN_POINT('Ctrl Pts',(-201.813823110784,64.7537534520113,11.4933050228246));
#17955=CARTESIAN_POINT('Ctrl Pts',(-203.06734588331,67.5450360698843,11.6522133416289));
#17956=CARTESIAN_POINT('Ctrl Pts',(-206.092704349143,68.0030580642296,11.8111216604332));
#17957=CARTESIAN_POINT('Ctrl Pts',(-208.11628368061,65.7079099898478,11.9700299792375));
#17958=CARTESIAN_POINT('Ctrl Pts',(-207.282888963754,62.763757948938,12.1289382980418));
#17959=CARTESIAN_POINT('Ctrl Pts',(-204.356567160304,61.869767626425,12.2878466168461));
#17960=CARTESIAN_POINT('Ctrl Pts',(-202.020137392775,63.8455393580491,12.4467549356504));
#17961=CARTESIAN_POINT('Ctrl Pts',(-202.415612358234,66.8797077030384,12.6056632544547));
#17962=CARTESIAN_POINT('Ctrl Pts',(-205.180425028513,68.1905810350019,12.764571573259));
#17963=CARTESIAN_POINT('Ctrl Pts',(-207.779826049193,66.5763653345084,12.9234798920633));
#17964=CARTESIAN_POINT('Ctrl Pts',(-207.830713617579,63.5169555141125,13.0823882108676));
#17965=CARTESIAN_POINT('Ctrl Pts',(-205.286434579534,61.8171843025619,13.241296529672));
#17966=CARTESIAN_POINT('Ctrl Pts',(-202.479555520672,63.0353829490269,13.4002048484763));
#17967=CARTESIAN_POINT('Ctrl Pts',(-201.983391789395,66.0547205491346,13.5591131672806));
#17968=CARTESIAN_POINT('Ctrl Pts',(-204.252820750779,68.1071021393641,13.7180214860849));
#17969=CARTESIAN_POINT('Ctrl Pts',(-207.207255294343,67.3109272132444,13.8769298048892));
#17970=CARTESIAN_POINT('Ctrl Pts',(-208.138102859107,64.3961200517564,14.0358381236935));
#17971=CARTESIAN_POINT('Ctrl Pts',(-206.191972786239,62.034943267128,14.1947464424978));
#17972=CARTESIAN_POINT('Ctrl Pts',(-203.153055406645,62.3920973764689,14.3536547613021));
#17973=CARTESIAN_POINT('Ctrl Pts',(-201.807396143545,65.1401474196413,14.5125630801064));
#17974=CARTESIAN_POINT('Ctrl Pts',(-203.388680503087,67.7597119642983,14.6714713989107));
#17975=CARTESIAN_POINT('Ctrl Pts',(-206.447204382496,67.8492032407486,14.830379717715));
#17976=CARTESIAN_POINT('Ctrl Pts',(-208.178947841049,65.3265772099636,14.9892880365193));
#17977=CARTESIAN_POINT('Ctrl Pts',(-206.996266663157,62.5045480630999,15.1481963553236));
#17978=CARTESIAN_POINT('Ctrl Pts',(-203.983432138862,61.9703229667084,15.3071046741279));
#17979=CARTESIAN_POINT('Ctrl Pts',(-201.902572335763,64.2136686064732,15.4660129929322));
#17980=CARTESIAN_POINT('Ctrl Pts',(-202.66140645512,67.1779208847556,15.6249213117366));
#17981=CARTESIAN_POINT('Ctrl Pts',(-205.564222877932,68.1454656278869,15.7838296305408));
#17982=CARTESIAN_POINT('Ctrl Pts',(-207.949795141323,66.2293114813142,15.9427379493452));
#17983=CARTESIAN_POINT('Ctrl Pts',(-207.630968346465,63.1860789341055,16.1016462681495));
#17984=CARTESIAN_POINT('Ctrl Pts',(-204.900222369535,61.805951176065,16.2605545869538));
#17985=CARTESIAN_POINT('Ctrl Pts',(-202.260697801607,63.353840056302,16.4194629057581));
#17986=CARTESIAN_POINT('Ctrl Pts',(-202.133056954791,66.4114280330604,16.5783712245624));
#17987=CARTESIAN_POINT('Ctrl Pts',(-204.632722473373,68.1739683102836,16.7372795433667));
#17988=CARTESIAN_POINT('Ctrl Pts',(-207.471316987812,67.0288605189738,16.896187862171));
#17989=CARTESIAN_POINT('Ctrl Pts',(-208.039624584823,64.0192083031125,17.0550961809753));
#17990=CARTESIAN_POINT('Ctrl Pts',(-206.56709509676,62.6211960514382,17.1610350601782));
#17991=CARTESIAN_POINT('Ctrl Pts',(-205.698066426161,62.3888678140614,17.2140044997796));
#17992=CARTESIAN_POINT('Ctrl Pts',(-207.195197104019,66.8768634390787,-0.214004499779621));
#17993=CARTESIAN_POINT('Ctrl Pts',(-207.819848796546,66.1462649533789,-0.161035060178185));
#17994=CARTESIAN_POINT('Ctrl Pts',(-208.270381695193,64.0238642990776,-0.0550961809753146));
#17995=CARTESIAN_POINT('Ctrl Pts',(-205.948234431212,61.7175191469019,0.103812137828992));
#17996=CARTESIAN_POINT('Ctrl Pts',(-202.755424311813,62.4272763820159,0.262720456633299));
#17997=CARTESIAN_POINT('Ctrl Pts',(-201.621026904811,65.4923916653317,0.421628775437605));
#17998=CARTESIAN_POINT('Ctrl Pts',(-203.584133015616,68.107677391492,0.580537094241912));
#17999=CARTESIAN_POINT('Ctrl Pts',(-206.845436332065,67.8731070036025,0.739445413046219));
#18000=CARTESIAN_POINT('Ctrl Pts',(-208.414793219705,65.004879314059,0.898353731850525));
#18001=CARTESIAN_POINT('Ctrl Pts',(-206.853540350764,62.131996121022,1.05726205065483));
#18002=CARTESIAN_POINT('Ctrl Pts',(-203.592965645672,61.88855533608,1.21617036945914));
#18003=CARTESIAN_POINT('Ctrl Pts',(-201.622352451459,64.4976092498449,1.37507868826345));
#18004=CARTESIAN_POINT('Ctrl Pts',(-202.748324823919,67.5672702726462,1.53398700706775));
#18005=CARTESIAN_POINT('Ctrl Pts',(-205.938609752273,68.2832764585058,1.69289532587206));
#18006=CARTESIAN_POINT('Ctrl Pts',(-208.268386817258,65.9892164116696,1.85180364467637));
#18007=CARTESIAN_POINT('Ctrl Pts',(-207.601743831544,62.7882514210722,2.01071196348067));
#18008=CARTESIAN_POINT('Ctrl Pts',(-204.549850960038,61.6149939701982,2.16962028228498));
#18009=CARTESIAN_POINT('Ctrl Pts',(-201.910649804104,63.545071649082,2.32852860108929));
#18010=CARTESIAN_POINT('Ctrl Pts',(-202.103730326783,66.8090116530371,2.48743691989359));
#18011=CARTESIAN_POINT('Ctrl Pts',(-204.952078540099,68.4144698591525,2.6463452386979));
#18012=CARTESIAN_POINT('Ctrl Pts',(-207.844360599983,66.8895803259649,2.80525355750221));
#18013=CARTESIAN_POINT('Ctrl Pts',(-208.128964658589,63.6323446379311,2.96416187630651));
#18014=CARTESIAN_POINT('Ctrl Pts',(-205.544968887098,61.6289601151182,3.12307019511082));
#18015=CARTESIAN_POINT('Ctrl Pts',(-202.461351732326,62.7161072739279,3.28197851391513));
#18016=CARTESIAN_POINT('Ctrl Pts',(-201.705138934727,65.8971017610087,3.44088683271943));
#18017=CARTESIAN_POINT('Ctrl Pts',(-203.969617936122,68.2556433785665,3.59979515152374));
#18018=CARTESIAN_POINT('Ctrl Pts',(-207.178739697151,67.629447535158,3.75870347032805));
#18019=CARTESIAN_POINT('Ctrl Pts',(-208.390417255234,64.592603579895,3.91761178913235));
#18020=CARTESIAN_POINT('Ctrl Pts',(-206.493798167673,61.9292561093994,4.07652010793666));
#18021=CARTESIAN_POINT('Ctrl Pts',(-203.227681615882,62.0811323166393,4.23542842674096));
#18022=CARTESIAN_POINT('Ctrl Pts',(-201.586406749804,64.908993792451,4.39433674554527));
#18023=CARTESIAN_POINT('Ctrl Pts',(-203.074676022485,67.8202887421631,4.55324506434958));
#18024=CARTESIAN_POINT('Ctrl Pts',(-206.328060798801,68.1459744948553,4.71215338315388));
#18025=CARTESIAN_POINT('Ctrl Pts',(-208.363894278238,65.5874659925654,4.8710617019582));
#18026=CARTESIAN_POINT('Ctrl Pts',(-207.315747080937,62.4903752342799,5.0299700207625));
#18027=CARTESIAN_POINT('Ctrl Pts',(-204.144548842459,61.6940804116484,5.18887833956681));
#18028=CARTESIAN_POINT('Ctrl Pts',(-201.757618664014,63.9286157180384,5.34778665837111));
#18029=CARTESIAN_POINT('Ctrl Pts',(-202.343267454975,67.14538415949,5.50669497717542));
#18030=CARTESIAN_POINT('Ctrl Pts',(-205.364578949465,68.3952883820365,5.66560329597973));
#18031=CARTESIAN_POINT('Ctrl Pts',(-208.051648537909,66.5324301643681,5.82451161478404));
#18032=CARTESIAN_POINT('Ctrl Pts',(-207.941000854442,63.2646570996623,5.98341993358834));
#18033=CARTESIAN_POINT('Ctrl Pts',(-205.134076458582,61.5878270104172,6.14232825239265));
#18034=CARTESIAN_POINT('Ctrl Pts',(-202.204232264038,63.0392389808696,6.30123657119695));
#18035=CARTESIAN_POINT('Ctrl Pts',(-201.837516682106,66.2882547386403,6.46014489000126));
#18036=CARTESIAN_POINT('Ctrl Pts',(-204.370130459597,68.3562129505824,6.61905320880557));
#18037=CARTESIAN_POINT('Ctrl Pts',(-207.480201591807,67.3472326411288,6.77796152760987));
#18038=CARTESIAN_POINT('Ctrl Pts',(-208.316451625349,64.1863356808223,6.93686984641418));
#18039=CARTESIAN_POINT('Ctrl Pts',(-206.112215876065,61.77139707418,7.09577816521849));
#18040=CARTESIAN_POINT('Ctrl Pts',(-202.888313042611,62.3164055445022,7.25468648402279));
#18041=CARTESIAN_POINT('Ctrl Pts',(-201.600381209803,65.3217034176442,7.4135948028271));
#18042=CARTESIAN_POINT('Ctrl Pts',(-203.429181887011,68.0320671931028,7.57250312163141));
#18043=CARTESIAN_POINT('Ctrl Pts',(-206.698091053498,67.9626656547127,7.73141144043571));
#18044=CARTESIAN_POINT('Ctrl Pts',(-208.410209321351,65.1771253571837,7.89031975924002));
#18045=CARTESIAN_POINT('Ctrl Pts',(-206.995885798594,62.229198511882,8.04922807804433));
#18046=CARTESIAN_POINT('Ctrl Pts',(-203.751756483289,61.8215115022116,8.20813639684863));
#18047=CARTESIAN_POINT('Ctrl Pts',(-201.652002872745,64.3278272220048,8.36704471565294));
#18048=CARTESIAN_POINT('Ctrl Pts',(-202.621655608597,67.4503834319279,8.52595303445724));
#18049=CARTESIAN_POINT('Ctrl Pts',(-205.771747900224,68.3264554988884,8.68486135326156));
#18050=CARTESIAN_POINT('Ctrl Pts',(-208.214310342592,66.1528703435735,8.84376967206586));
#18051=CARTESIAN_POINT('Ctrl Pts',(-207.710028988554,62.9223465426638,9.00267799087016));
#18052=CARTESIAN_POINT('Ctrl Pts',(-204.721223347243,61.5965922099369,9.16158630967448));
#18053=CARTESIAN_POINT('Ctrl Pts',(-201.987997025351,63.3910440999545,9.32049462847878));
#18054=CARTESIAN_POINT('Ctrl Pts',(-202.016141366082,66.6605687761665,9.47940294728308));
#18055=CARTESIAN_POINT('Ctrl Pts',(-204.779853952418,68.4077025582228,9.63831126608739));
#18056=CARTESIAN_POINT('Ctrl Pts',(-207.74539397465,67.0306927220875,9.7972195848917));
#18057=CARTESIAN_POINT('Ctrl Pts',(-208.193987485624,63.7919664949749,9.95612790369601));
#18058=CARTESIAN_POINT('Ctrl Pts',(-205.714368968315,61.6607518833287,10.1150362225003));
#18059=CARTESIAN_POINT('Ctrl Pts',(-202.579824965209,62.5909226229609,10.2739445413046));
#18060=CARTESIAN_POINT('Ctrl Pts',(-201.664070384204,65.7297085761028,10.4328528601089));
#18061=CARTESIAN_POINT('Ctrl Pts',(-203.806658789964,68.1995058624756,10.5917611789132));
#18062=CARTESIAN_POINT('Ctrl Pts',(-207.043289079357,67.7360319343462,10.7506694977175));
#18063=CARTESIAN_POINT('Ctrl Pts',(-208.406654778216,64.7641945088715,10.9095778165218));
#18064=CARTESIAN_POINT('Ctrl Pts',(-206.646837451881,62.0085409221143,11.0684861353262));
#18065=CARTESIAN_POINT('Ctrl Pts',(-203.377217956024,61.9954235830429,11.2273944541305));
#18066=CARTESIAN_POINT('Ctrl Pts',(-201.595346900585,64.7368683215086,11.3863027729348));
#18067=CARTESIAN_POINT('Ctrl Pts',(-202.934823753585,67.7195492418465,11.5452110917391));
#18068=CARTESIAN_POINT('Ctrl Pts',(-206.167631107251,68.2089778130996,11.7041194105434));
#18069=CARTESIAN_POINT('Ctrl Pts',(-208.32996731216,65.7564513913839,11.8630277293477));
#18070=CARTESIAN_POINT('Ctrl Pts',(-207.439426703638,62.6104187887493,12.021936048152));
#18071=CARTESIAN_POINT('Ctrl Pts',(-204.312446958186,61.6551275327322,12.1808443669563));
#18072=CARTESIAN_POINT('Ctrl Pts',(-201.815808156835,63.7663779697622,12.3397526857606));
#18073=CARTESIAN_POINT('Ctrl Pts',(-202.238400848236,67.0085992961677,12.4986610045649));
#18074=CARTESIAN_POINT('Ctrl Pts',(-205.192796776167,68.4093592375623,12.6575693233692));
#18075=CARTESIAN_POINT('Ctrl Pts',(-207.970438774524,66.6844567356291,12.8164776421735));
#18076=CARTESIAN_POINT('Ctrl Pts',(-208.024815704448,63.4152631253657,12.9753859609778));
#18077=CARTESIAN_POINT('Ctrl Pts',(-205.306075404128,61.5989385693468,13.1342942797821));
#18078=CARTESIAN_POINT('Ctrl Pts',(-202.306728594544,62.9006691202864,13.2932025985865));
#18079=CARTESIAN_POINT('Ctrl Pts',(-201.776542906729,66.1270427573506,13.4521109173907));
#18080=CARTESIAN_POINT('Ctrl Pts',(-204.201586655377,68.3201561924549,13.6110192361951));
#18081=CARTESIAN_POINT('Ctrl Pts',(-207.35860683207,67.4693875364316,13.7699275549993));
#18082=CARTESIAN_POINT('Ctrl Pts',(-208.353282632143,64.3547119921617,13.9288358738037));
#18083=CARTESIAN_POINT('Ctrl Pts',(-206.273706382977,61.8316292702757,14.087744192608));
#18084=CARTESIAN_POINT('Ctrl Pts',(-203.026410380573,62.2132734437214,14.2466525114123));
#18085=CARTESIAN_POINT('Ctrl Pts',(-201.588479236079,65.1497573308851,14.4055608302166));
#18086=CARTESIAN_POINT('Ctrl Pts',(-203.278192294382,67.9489454664442,14.5644691490209));
#18087=CARTESIAN_POINT('Ctrl Pts',(-206.546439214669,68.0445731614314,14.7233774678252));
#18088=CARTESIAN_POINT('Ctrl Pts',(-208.396928355277,65.3489706154936,14.8822857866295));
#18089=CARTESIAN_POINT('Ctrl Pts',(-207.133150706409,62.3334348760842,15.0411941054338));
#18090=CARTESIAN_POINT('Ctrl Pts',(-203.913726061192,61.7625779546212,15.2001024242381));
#18091=CARTESIAN_POINT('Ctrl Pts',(-201.690181661616,64.1597498477878,15.3590107430424));
#18092=CARTESIAN_POINT('Ctrl Pts',(-202.501049051044,67.3272609614558,15.5179190618467));
#18093=CARTESIAN_POINT('Ctrl Pts',(-205.602911651457,68.361150266119,15.6768273806511));
#18094=CARTESIAN_POINT('Ctrl Pts',(-208.152062650551,66.3136053930871,15.8357356994553));
#18095=CARTESIAN_POINT('Ctrl Pts',(-207.811373896275,63.0616983319427,15.9946440182597));
#18096=CARTESIAN_POINT('Ctrl Pts',(-204.893380615506,61.5869351871512,16.153552337064));
#18097=CARTESIAN_POINT('Ctrl Pts',(-202.0728637975,63.240962837495,16.3124606558683));
#18098=CARTESIAN_POINT('Ctrl Pts',(-201.936470615377,66.5082096802679,16.4713689746726));
#18099=CARTESIAN_POINT('Ctrl Pts',(-204.607538246351,68.3916073779926,16.6302772934769));
#18100=CARTESIAN_POINT('Ctrl Pts',(-207.640775240907,67.167979523543,16.7891856122812));
#18101=CARTESIAN_POINT('Ctrl Pts',(-208.248051700709,63.9519553977084,16.9480939310855));
#18102=CARTESIAN_POINT('Ctrl Pts',(-206.674550837501,62.4580814192127,17.0540328102884));
#18103=CARTESIAN_POINT('Ctrl Pts',(-205.745932854347,62.2098224301579,17.1070022498898));
#18104=CARTESIAN_POINT('Ctrl Pts',(-207.336062657696,66.9973015569306,-0.321006749669432));
#18105=CARTESIAN_POINT('Ctrl Pts',(-208.000798179763,66.2198206477731,-0.268037310067996));
#18106=CARTESIAN_POINT('Ctrl Pts',(-208.480241724338,63.9612257798655,-0.162098430865125));
#18107=CARTESIAN_POINT('Ctrl Pts',(-206.009082529054,61.5068827161415,-0.00319011206081843));
#18108=CARTESIAN_POINT('Ctrl Pts',(-202.61139013989,62.2621849939844,0.155718206743488));
#18109=CARTESIAN_POINT('Ctrl Pts',(-201.404198577622,65.5239883836563,0.314626525547794));
#18110=CARTESIAN_POINT('Ctrl Pts',(-203.493276988919,68.3070967035895,0.473534844352101));
#18111=CARTESIAN_POINT('Ctrl Pts',(-206.96385777596,68.0574739600344,0.632443163156408));
#18112=CARTESIAN_POINT('Ctrl Pts',(-208.633920120295,65.0051924190987,0.791351481960715));
#18113=CARTESIAN_POINT('Ctrl Pts',(-206.972481828636,61.9479566315291,0.95025980076502));
#18114=CARTESIAN_POINT('Ctrl Pts',(-203.502676407862,61.6888942785303,1.10916811956933));
#18115=CARTESIAN_POINT('Ctrl Pts',(-201.405609184451,64.4653708913607,1.26807643837363));
#18116=CARTESIAN_POINT('Ctrl Pts',(-202.603835078648,67.7320117201147,1.42698475717794));
#18117=CARTESIAN_POINT('Ctrl Pts',(-205.998840235539,68.4939639431765,1.58589307598225));
#18118=CARTESIAN_POINT('Ctrl Pts',(-208.478118835308,66.0526943186335,1.74480139478656));
#18119=CARTESIAN_POINT('Ctrl Pts',(-207.768697443447,62.6463237610936,1.90370971359086));
#18120=CARTESIAN_POINT('Ctrl Pts',(-204.520964946279,61.3977785102674,2.06261803239517));
#18121=CARTESIAN_POINT('Ctrl Pts',(-201.712406546107,63.4517090588448,2.22152635119947));
#18122=CARTESIAN_POINT('Ctrl Pts',(-201.917877024422,66.9250957293356,2.38043467000378));
#18123=CARTESIAN_POINT('Ctrl Pts',(-204.949003425354,68.6335760097311,2.53934298880809));
#18124=CARTESIAN_POINT('Ctrl Pts',(-208.026882902896,67.010834485032,2.6982513076124));
#18125=CARTESIAN_POINT('Ctrl Pts',(-208.329749972245,63.5445823456684,2.8571596264167));
#18126=CARTESIAN_POINT('Ctrl Pts',(-205.579939479888,61.4126408611514,3.01606794522101));
#18127=CARTESIAN_POINT('Ctrl Pts',(-202.298446955729,62.5695501320622,3.17497626402532));
#18128=CARTESIAN_POINT('Ctrl Pts',(-201.493708067131,65.9546686810988,3.33388458282962));
#18129=CARTESIAN_POINT('Ctrl Pts',(-203.90349843384,68.4645576515751,3.49279290163393));
#18130=CARTESIAN_POINT('Ctrl Pts',(-207.318549180862,67.7981788906371,3.65170122043823));
#18131=CARTESIAN_POINT('Ctrl Pts',(-208.607979952898,64.5664609969902,3.81060953924254));
#18132=CARTESIAN_POINT('Ctrl Pts',(-206.589655029722,61.7322068159406,3.96951785804685));
#18133=CARTESIAN_POINT('Ctrl Pts',(-203.113952142563,61.893828902484,4.12842617685116));
#18134=CARTESIAN_POINT('Ctrl Pts',(-201.367356851125,64.9031539342483,4.28733449565546));
#18135=CARTESIAN_POINT('Ctrl Pts',(-202.951128197279,68.0012663566409,4.44624281445977));
#18136=CARTESIAN_POINT('Ctrl Pts',(-206.413282312349,68.3478513278105,4.60515113326408));
#18137=CARTESIAN_POINT('Ctrl Pts',(-208.579754999423,65.6251636198798,4.76405945206838));
#18138=CARTESIAN_POINT('Ctrl Pts',(-207.464348313206,62.3293328925706,4.92296777087269));
#18139=CARTESIAN_POINT('Ctrl Pts',(-204.089654636955,61.4819399198572,5.081876089677));
#18140=CARTESIAN_POINT('Ctrl Pts',(-201.549555414801,63.8598651079893,5.2407844084813));
#18141=CARTESIAN_POINT('Ctrl Pts',(-202.172785223452,67.2830532220644,5.39969272728561));
#18142=CARTESIAN_POINT('Ctrl Pts',(-205.387973940047,68.613163659365,5.55860104608992));
#18143=CARTESIAN_POINT('Ctrl Pts',(-208.247472484712,66.6307660373427,5.71750936489423));
#18144=CARTESIAN_POINT('Ctrl Pts',(-208.129724551721,63.1533003390197,5.87641768369853));
#18145=CARTESIAN_POINT('Ctrl Pts',(-205.142680129997,61.368868249703,6.03532600250284));
#18146=CARTESIAN_POINT('Ctrl Pts',(-202.024828159798,62.9134171646498,6.19423432130715));
#18147=CARTESIAN_POINT('Ctrl Pts',(-201.634580479816,66.3709219017407,6.35314264011145));
#18148=CARTESIAN_POINT('Ctrl Pts',(-204.32971180134,68.5715807618264,6.51205095891576));
#18149=CARTESIAN_POINT('Ctrl Pts',(-207.639355851724,67.4978542982895,6.67095927772006));
#18150=CARTESIAN_POINT('Ctrl Pts',(-208.529267956781,64.1341229320817,6.82986759652437));
#18151=CARTESIAN_POINT('Ctrl Pts',(-206.18358664496,61.5642179840126,6.98877591532868));
#18152=CARTESIAN_POINT('Ctrl Pts',(-202.752806325743,62.1441995871754,7.14768423413298));
#18153=CARTESIAN_POINT('Ctrl Pts',(-201.382228050665,65.3423470901251,7.30659255293729));
#18154=CARTESIAN_POINT('Ctrl Pts',(-203.328382663649,68.2266346071907,7.4655008717416));
#18155=CARTESIAN_POINT('Ctrl Pts',(-206.807057367278,68.1527795798118,7.62440919054589));
#18156=CARTESIAN_POINT('Ctrl Pts',(-208.629042073693,65.1884914716269,7.78331750935022));
#18157=CARTESIAN_POINT('Ctrl Pts',(-207.123961567999,62.0513964889848,7.94222582815451));
#18158=CARTESIAN_POINT('Ctrl Pts',(-203.671656835844,61.6175482493094,8.10113414695882));
#18159=CARTESIAN_POINT('Ctrl Pts',(-201.437162269969,64.2846939697036,8.26004246576313));
#18160=CARTESIAN_POINT('Ctrl Pts',(-202.469037513887,67.6076242638456,8.41895078456743));
#18161=CARTESIAN_POINT('Ctrl Pts',(-205.821270877028,68.5399137777715,8.57785910337175));
#18162=CARTESIAN_POINT('Ctrl Pts',(-208.420572279286,66.2268499051207,8.73676742217605));
#18163=CARTESIAN_POINT('Ctrl Pts',(-207.883931246923,62.7890237517031,8.89567574098036));
#18164=CARTESIAN_POINT('Ctrl Pts',(-204.703334280485,61.3781959110996,9.05458405978466));
#18165=CARTESIAN_POINT('Ctrl Pts',(-201.794717129927,63.2877975790446,9.21349237858897));
#18166=CARTESIAN_POINT('Ctrl Pts',(-201.824667489868,66.7671272895889,9.37240069739327));
#18167=CARTESIAN_POINT('Ctrl Pts',(-204.765727205063,68.6263744518545,9.53130901619758));
#18168=CARTESIAN_POINT('Ctrl Pts',(-207.921565600238,67.1610020478975,9.69021733500189));
#18169=CARTESIAN_POINT('Ctrl Pts',(-208.398945306849,63.714447119501,9.84912565380619));
#18170=CARTESIAN_POINT('Ctrl Pts',(-205.76020994545,61.4464727035873,10.0080339726105));
#18171=CARTESIAN_POINT('Ctrl Pts',(-202.424522602772,62.4363323959849,10.1669422914148));
#18172=CARTESIAN_POINT('Ctrl Pts',(-201.450004152294,65.7765338941607,10.3258506102191));
#18173=CARTESIAN_POINT('Ctrl Pts',(-203.730082217424,68.4048177973288,10.4847589290234));
#18174=CARTESIAN_POINT('Ctrl Pts',(-207.174406712011,67.9116027988503,10.6436672478277));
#18175=CARTESIAN_POINT('Ctrl Pts',(-208.625259435921,64.7490628967685,10.802575566632));
#18176=CARTESIAN_POINT('Ctrl Pts',(-206.752514827754,61.816579326257,10.9614838854363));
#18177=CARTESIAN_POINT('Ctrl Pts',(-203.273084212998,61.8026202489985,11.1203922042406));
#18178=CARTESIAN_POINT('Ctrl Pts',(-201.376870690385,64.7199831910058,11.279300523045));
#18179=CARTESIAN_POINT('Ctrl Pts',(-202.80230162386,67.8940624138088,11.4382088418493));
#18180=CARTESIAN_POINT('Ctrl Pts',(-206.24255786536,68.4148975619695,11.5971171606536));
#18181=CARTESIAN_POINT('Ctrl Pts',(-208.54365094371,65.80499279292,11.7560254794579));
#18182=CARTESIAN_POINT('Ctrl Pts',(-207.595964443522,62.4570796285605,11.9149337982622));
#18183=CARTESIAN_POINT('Ctrl Pts',(-204.268326756069,61.4404874390394,12.0738421170665));
#18184=CARTESIAN_POINT('Ctrl Pts',(-201.611478920896,63.6872165814752,12.2327504358708));
#18185=CARTESIAN_POINT('Ctrl Pts',(-202.061189338237,67.1374908892971,12.3916587546751));
#18186=CARTESIAN_POINT('Ctrl Pts',(-205.205168523821,68.6281374401227,12.5505670734794));
#18187=CARTESIAN_POINT('Ctrl Pts',(-208.161051499856,66.7925481367497,12.7094753922837));
#18188=CARTESIAN_POINT('Ctrl Pts',(-208.218917791317,63.3135707366188,12.868383711088));
#18189=CARTESIAN_POINT('Ctrl Pts',(-205.325716228722,61.3806928361316,13.0272920298923));
#18190=CARTESIAN_POINT('Ctrl Pts',(-202.133901668416,62.7659552915461,13.1862003486966));
#18191=CARTESIAN_POINT('Ctrl Pts',(-201.569694024063,66.1993649655665,13.3451086675009));
#18192=CARTESIAN_POINT('Ctrl Pts',(-204.150352559975,68.5332102455456,13.5040169863053));
#18193=CARTESIAN_POINT('Ctrl Pts',(-207.509958369796,67.627847859619,13.6629253051095));
#18194=CARTESIAN_POINT('Ctrl Pts',(-208.568462405179,64.313303932567,13.8218336239139));
#18195=CARTESIAN_POINT('Ctrl Pts',(-206.355439979715,61.6283152734234,13.9807419427182));
#18196=CARTESIAN_POINT('Ctrl Pts',(-202.899765354501,62.0344495109738,14.1396502615225));
#18197=CARTESIAN_POINT('Ctrl Pts',(-201.369562328613,65.1593672421288,14.2985585803268));
#18198=CARTESIAN_POINT('Ctrl Pts',(-203.167704085678,68.1381789685902,14.4574668991311));
#18199=CARTESIAN_POINT('Ctrl Pts',(-206.645674046841,68.2399430821141,14.6163752179354));
#18200=CARTESIAN_POINT('Ctrl Pts',(-208.614908869506,65.3713640210235,14.7752835367397));
#18201=CARTESIAN_POINT('Ctrl Pts',(-207.270034749662,62.1623216890685,14.934191855544));
#18202=CARTESIAN_POINT('Ctrl Pts',(-203.844019983521,61.5548329425339,15.0931001743483));
#18203=CARTESIAN_POINT('Ctrl Pts',(-201.47779098747,64.1058310891023,15.2520084931526));
#18204=CARTESIAN_POINT('Ctrl Pts',(-202.340691646968,67.4766010381562,15.4109168119569));
#18205=CARTESIAN_POINT('Ctrl Pts',(-205.641600424982,68.5768349043511,15.5698251307612));
#18206=CARTESIAN_POINT('Ctrl Pts',(-208.354330159779,66.3978993048601,15.7287334495655));
#18207=CARTESIAN_POINT('Ctrl Pts',(-207.991779446085,62.9373177297799,15.8876417683699));
#18208=CARTESIAN_POINT('Ctrl Pts',(-204.886538861478,61.3679191982373,16.0465500871742));
#18209=CARTESIAN_POINT('Ctrl Pts',(-201.885029793392,63.1280856186881,16.2054584059785));
#18210=CARTESIAN_POINT('Ctrl Pts',(-201.739884275964,66.6049913274753,16.3643667247828));
#18211=CARTESIAN_POINT('Ctrl Pts',(-204.58235401933,68.6092464457014,16.5232750435871));
#18212=CARTESIAN_POINT('Ctrl Pts',(-207.810233494003,67.3070985281123,16.6821833623914));
#18213=CARTESIAN_POINT('Ctrl Pts',(-208.456478816595,63.8847024923042,16.8410916811957));
#18214=CARTESIAN_POINT('Ctrl Pts',(-206.782006578242,62.2949667869872,16.9470305603986));
#18215=CARTESIAN_POINT('Ctrl Pts',(-205.793799282533,62.0307770462544,17.));
#18216=CARTESIAN_POINT('Ctrl Pts',(-206.913465996665,66.6359872033749,0.));
#18217=CARTESIAN_POINT('Ctrl Pts',(-206.975064353962,66.5780998731382,1.31385826762081E-17));
#18218=CARTESIAN_POINT('Ctrl Pts',(-207.033290473413,66.517061027268,-9.08596571292744E-17));
#18219=CARTESIAN_POINT('Ctrl Pts',(-207.088148064904,66.4532556948983,-9.36750677027476E-17));
#18220=CARTESIAN_POINT('Ctrl Pts',(-207.144459507376,66.3877593760565,-9.65650930617943E-17));
#18221=CARTESIAN_POINT('Ctrl Pts',(-207.197221943433,66.3193475595673,1.65439813454464E-17));
#18222=CARTESIAN_POINT('Ctrl Pts',(-207.246413817218,66.2483881525801,-6.24500451351651E-17));
#18223=CARTESIAN_POINT('Ctrl Pts',(-207.297364147824,66.1748921670169,-1.44267862903041E-16));
#18224=CARTESIAN_POINT('Ctrl Pts',(-207.344484671467,66.0986626833147,-2.11570137502538E-16));
#18225=CARTESIAN_POINT('Ctrl Pts',(-207.387716349603,66.0200643070203,-1.45716771982052E-16));
#18226=CARTESIAN_POINT('Ctrl Pts',(-207.406630208787,65.9856775173915,-1.16905924566839E-16));
#18227=CARTESIAN_POINT('Ctrl Pts',(-207.424799222197,65.950836798184,4.63322983862409E-16));
#18228=CARTESIAN_POINT('Ctrl Pts',(-207.442215989061,65.9155705830685,5.06539254985228E-16));
#18229=CARTESIAN_POINT('Ctrl Pts',(-207.451672386856,65.8964228640095,5.30003440623795E-16));
#18230=CARTESIAN_POINT('Ctrl Pts',(-207.460907000843,65.8771496923497,-3.05997193293947E-17));
#18231=CARTESIAN_POINT('Ctrl Pts',(-207.46991844596,65.8577554924582,-2.77555756156289E-17));
#18232=CARTESIAN_POINT('Ctrl Pts',(-207.478568341098,65.839139411115,-2.50255423570532E-17));
#18233=CARTESIAN_POINT('Ctrl Pts',(-207.487015107733,65.8204058124637,-3.76747677011534E-16));
#18234=CARTESIAN_POINT('Ctrl Pts',(-207.495243417805,65.8015914143888,-3.60822483003176E-16));
#18235=CARTESIAN_POINT('Ctrl Pts',(-207.53178628096,65.7180345274726,-2.90096880750225E-16));
#18236=CARTESIAN_POINT('Ctrl Pts',(-207.564069677878,65.6327939693891,9.41786769087706E-16));
#18237=CARTESIAN_POINT('Ctrl Pts',(-207.592069998968,65.5462689644831,8.32667268468867E-16));
#18238=CARTESIAN_POINT('Ctrl Pts',(-207.620534587111,65.4583093078501,7.21738481850149E-16));
#18239=CARTESIAN_POINT('Ctrl Pts',(-207.644573379561,65.3690215011792,1.52679044846908E-16));
#18240=CARTESIAN_POINT('Ctrl Pts',(-207.664122455327,65.278787817363,1.80411241501588E-16));
#18241=CARTESIAN_POINT('Ctrl Pts',(-207.683373891228,65.1899279653208,2.07721208105181E-16));
#18242=CARTESIAN_POINT('Ctrl Pts',(-207.698271558591,65.1001499107623,4.03184391054926E-16));
#18243=CARTESIAN_POINT('Ctrl Pts',(-207.7087114019,65.0097957225238,4.16333634234434E-16));
#18244=CARTESIAN_POINT('Ctrl Pts',(-207.712805706108,64.9743605610785,4.21490512559996E-16));
#18245=CARTESIAN_POINT('Ctrl Pts',(-207.716213877993,64.9388366075109,3.54060526755959E-16));
#18246=CARTESIAN_POINT('Ctrl Pts',(-207.718927650427,64.9032439712385,4.02455846426619E-16));
#18247=CARTESIAN_POINT('Ctrl Pts',(-207.720523480385,64.8823137729101,4.30914644227349E-16));
#18248=CARTESIAN_POINT('Ctrl Pts',(-207.721879164357,64.8613598200859,1.01489021387037E-17));
#18249=CARTESIAN_POINT('Ctrl Pts',(-207.722992828189,64.8403861801911,-1.38777878078145E-17));
#18250=CARTESIAN_POINT('Ctrl Pts',(-207.723754506584,64.826041484871,-3.03105838585251E-17));
#18251=CARTESIAN_POINT('Ctrl Pts',(-207.724402910459,64.8116871985238,1.32396209708937E-16));
#18252=CARTESIAN_POINT('Ctrl Pts',(-207.724937054538,64.7973399810991,1.38777878078145E-16));
#18253=CARTESIAN_POINT('Ctrl Pts',(-207.728480924081,64.7021509323424,1.81118139856045E-16));
#18254=CARTESIAN_POINT('Ctrl Pts',(-207.727008512663,64.6071119050743,-3.51651214267614E-17));
#18255=CARTESIAN_POINT('Ctrl Pts',(-207.720461908733,64.5126221906688,-2.77555756156289E-17));
#18256=CARTESIAN_POINT('Ctrl Pts',(-207.713937327651,64.4184503406908,-2.03709555972342E-17));
#18257=CARTESIAN_POINT('Ctrl Pts',(-207.702372994406,64.3248231595109,-6.60606084003931E-17));
#18258=CARTESIAN_POINT('Ctrl Pts',(-207.685663588442,64.2321180011441,-5.55111512312578E-17));
#18259=CARTESIAN_POINT('Ctrl Pts',(-207.683580824393,64.2205626549263,-5.41962014253678E-17));
#18260=CARTESIAN_POINT('Ctrl Pts',(-207.68141805756,64.2090216217805,-4.52545427453158E-17));
#18261=CARTESIAN_POINT('Ctrl Pts',(-207.679175027131,64.1974956243958,-5.55111512312578E-17));
#18262=CARTESIAN_POINT('Ctrl Pts',(-207.661554797347,64.1069526162377,-1.64870956444071E-16));
#18263=CARTESIAN_POINT('Ctrl Pts',(-207.638985905053,64.0173371417335,4.55048391484254E-16));
#18264=CARTESIAN_POINT('Ctrl Pts',(-207.611743404672,63.9288865787528,5.27355936696949E-16));
#18265=CARTESIAN_POINT('Ctrl Pts',(-207.600816806121,63.8934102539034,5.56357515393362E-16));
#18266=CARTESIAN_POINT('Ctrl Pts',(-207.589137769353,63.858121381592,2.22458913192123E-16));
#18267=CARTESIAN_POINT('Ctrl Pts',(-207.576721747478,63.823035642348,2.22044604925031E-16));
#18268=CARTESIAN_POINT('Ctrl Pts',(-207.570942626356,63.806704748379,2.21851762347786E-16));
#18269=CARTESIAN_POINT('Ctrl Pts',(-207.565003819633,63.7904178674733,1.86961011374093E-16));
#18270=CARTESIAN_POINT('Ctrl Pts',(-207.55890679455,63.7741766065144,1.94289029309402E-16));
#18271=CARTESIAN_POINT('Ctrl Pts',(-207.553840826645,63.7606818766017,2.00377819033484E-16));
#18272=CARTESIAN_POINT('Ctrl Pts',(-207.548668946019,63.7472275150126,-2.33100565213495E-16));
#18273=CARTESIAN_POINT('Ctrl Pts',(-207.543393212818,63.7338163202487,-2.22044604925031E-16));
#18274=CARTESIAN_POINT('Ctrl Pts',(-207.509159730858,63.6467929859398,-1.50304051959292E-16));
#18275=CARTESIAN_POINT('Ctrl Pts',(-207.4705477531,63.5615605760055,2.94289231251776E-17));
#18276=CARTESIAN_POINT('Ctrl Pts',(-207.42788979993,63.4783502782173,-2.77555756156289E-17));
#18277=CARTESIAN_POINT('Ctrl Pts',(-207.383652831604,63.3920598907493,-8.70568001595249E-17));
#18278=CARTESIAN_POINT('Ctrl Pts',(-207.335064684792,63.3079433607353,2.06427004750576E-16));
#18279=CARTESIAN_POINT('Ctrl Pts',(-207.282440228002,63.2262620943519,1.66533453693773E-16));
#18280=CARTESIAN_POINT('Ctrl Pts',(-207.229239513817,63.143686387689,1.2620305339923E-16));
#18281=CARTESIAN_POINT('Ctrl Pts',(-207.171913188856,63.0635987542449,7.73907681327724E-17));
#18282=CARTESIAN_POINT('Ctrl Pts',(-207.110734970838,62.9862846789063,0.));
#18283=CARTESIAN_POINT('Ctrl Pts',(-207.08664473883,62.9558406079157,-3.04742704188559E-17));
#18284=CARTESIAN_POINT('Ctrl Pts',(-207.061956723682,62.9258268275662,6.15201622997646E-17));
#18285=CARTESIAN_POINT('Ctrl Pts',(-207.036685701927,62.8962618494865,5.55111512312578E-17));
#18286=CARTESIAN_POINT('Ctrl Pts',(-207.022377248651,62.8795221580103,5.21088489839094E-17));
#18287=CARTESIAN_POINT('Ctrl Pts',(-207.007881874863,62.8629263573898,1.92101835007536E-16));
#18288=CARTESIAN_POINT('Ctrl Pts',(-206.993202121486,62.8464779169567,1.94289029309402E-16));
#18289=CARTESIAN_POINT('Ctrl Pts',(-206.979146903046,62.8307292584226,1.96383171690125E-16));
#18290=CARTESIAN_POINT('Ctrl Pts',(-206.96491979389,62.8151127633992,1.78167578031119E-16));
#18291=CARTESIAN_POINT('Ctrl Pts',(-206.950542135111,62.7996517246072,1.66533453693773E-16));
#18292=CARTESIAN_POINT('Ctrl Pts',(-206.881823170714,62.7257546742894,1.10927392346557E-16));
#18293=CARTESIAN_POINT('Ctrl Pts',(-206.809592952989,62.6553193670047,2.26493089832809E-16));
#18294=CARTESIAN_POINT('Ctrl Pts',(-206.734165057036,62.5886325600171,2.22044604925031E-16));
#18295=CARTESIAN_POINT('Ctrl Pts',(-206.669049633309,62.5310631470145,2.18204315121696E-16));
#18296=CARTESIAN_POINT('Ctrl Pts',(-206.601550089891,62.476287232394,-5.66442745991914E-17));
#18297=CARTESIAN_POINT('Ctrl Pts',(-206.53184161149,62.4245048556646,0.));
#18298=CARTESIAN_POINT('Ctrl Pts',(-206.504681474983,62.4043291689635,2.20700016087845E-17));
#18299=CARTESIAN_POINT('Ctrl Pts',(-206.477185765765,62.3846081125284,1.56807690272953E-16));
#18300=CARTESIAN_POINT('Ctrl Pts',(-206.449363978737,62.3653543217963,1.66533453693773E-16));
#18301=CARTESIAN_POINT('Ctrl Pts',(-206.434093585115,62.3547865979153,1.71871580808257E-16));
#18302=CARTESIAN_POINT('Ctrl Pts',(-206.418726217455,62.3443606145378,-1.45925441287982E-16));
#18303=CARTESIAN_POINT('Ctrl Pts',(-206.403273624565,62.3340849578763,-1.11022302462516E-16));
#18304=CARTESIAN_POINT('Ctrl Pts',(-206.316688826831,62.2765078470346,8.4548838057753E-17));
#18305=CARTESIAN_POINT('Ctrl Pts',(-206.22734730699,62.2235888009188,7.07438163739693E-17));
#18306=CARTESIAN_POINT('Ctrl Pts',(-206.135559047579,62.1756508392814,-1.11022302462516E-16));
#18307=CARTESIAN_POINT('Ctrl Pts',(-206.043770788168,62.127712877644,-2.92788421299001E-16));
#18308=CARTESIAN_POINT('Ctrl Pts',(-205.949535136959,62.0847550816221,-2.90501423862547E-16));
#18309=CARTESIAN_POINT('Ctrl Pts',(-205.853123850132,62.0471417176263,-3.33066907387547E-16));
#18310=CARTESIAN_POINT('Ctrl Pts',(-205.834023263537,62.0396899208525,-3.41271880709564E-16));
#18311=CARTESIAN_POINT('Ctrl Pts',(-205.814837181401,62.0324480470172,-1.75194258867014E-16));
#18312=CARTESIAN_POINT('Ctrl Pts',(-205.795568724168,62.0254151527766,-1.66533453693773E-16));
#18313=CARTESIAN_POINT('Ctrl Pts',(-202.480291681284,64.9980775076607,1.61258330249194));
#18314=CARTESIAN_POINT('Ctrl Pts',(-202.479246282523,64.8744702547577,1.60474993100897));
#18315=CARTESIAN_POINT('Ctrl Pts',(-202.487554291616,64.7510041347843,1.596916559526));
#18316=CARTESIAN_POINT('Ctrl Pts',(-202.505700729609,64.6290014493569,1.58908318804303));
#18317=CARTESIAN_POINT('Ctrl Pts',(-202.628407364081,63.804016461602,1.53611374844159));
#18318=CARTESIAN_POINT('Ctrl Pts',(-203.200975742687,63.0459469563907,1.48314430884016));
#18319=CARTESIAN_POINT('Ctrl Pts',(-203.960945477611,62.7022784785898,1.43017486923872));
#18320=CARTESIAN_POINT('Ctrl Pts',(-204.720915212535,62.3586100007889,1.37720542963728));
#18321=CARTESIAN_POINT('Ctrl Pts',(-205.668286303777,62.4293425503984,1.32423599003585));
#18322=CARTESIAN_POINT('Ctrl Pts',(-206.368785519983,62.8820718258651,1.27126655043441));
#18323=CARTESIAN_POINT('Ctrl Pts',(-207.069284736189,63.3348011013318,1.21829711083298));
#18324=CARTESIAN_POINT('Ctrl Pts',(-207.522912077358,64.1695271026556,1.16532767123154));
#18325=CARTESIAN_POINT('Ctrl Pts',(-207.521734752234,65.0035767677775,1.11235823163011));
#18326=CARTESIAN_POINT('Ctrl Pts',(-207.52055742711,65.8376264328994,1.05938879202867));
#18327=CARTESIAN_POINT('Ctrl Pts',(-207.064575435692,66.6709997618192,1.00641935242723));
#18328=CARTESIAN_POINT('Ctrl Pts',(-206.362793044106,67.1217640390388,0.953449912825799));
#18329=CARTESIAN_POINT('Ctrl Pts',(-205.66101065252,67.5725283162583,0.900480473224363));
#18330=CARTESIAN_POINT('Ctrl Pts',(-204.713427860765,67.6406835417775,0.847511033622928));
#18331=CARTESIAN_POINT('Ctrl Pts',(-203.954442879917,67.2948210647681,0.794541594021492));
#18332=CARTESIAN_POINT('Ctrl Pts',(-203.195457899069,66.9489585877586,0.741572154420057));
#18333=CARTESIAN_POINT('Ctrl Pts',(-202.625070729129,66.1890784082204,0.688602714818621));
#18334=CARTESIAN_POINT('Ctrl Pts',(-202.504678660237,65.3638484733508,0.635633275217186));
#18335=CARTESIAN_POINT('Ctrl Pts',(-202.487215547386,65.2441472038771,0.627949950975436));
#18336=CARTESIAN_POINT('Ctrl Pts',(-202.47922037136,65.1230709697569,0.620266626733685));
#18337=CARTESIAN_POINT('Ctrl Pts',(-202.480232429385,65.0018635099461,0.612583302491936));
#18338=CARTESIAN_POINT('Ctrl Pts',(-204.206200717467,62.0307770462543,-5.55111512312578E-16));
#18339=CARTESIAN_POINT('Ctrl Pts',(-203.217993421758,62.2949667869871,0.052969439601435));
#18340=CARTESIAN_POINT('Ctrl Pts',(-201.543521124928,63.884702084602,0.158908318804306));
#18341=CARTESIAN_POINT('Ctrl Pts',(-202.189766556512,67.3070986306701,0.317816637608613));
#18342=CARTESIAN_POINT('Ctrl Pts',(-205.417645976078,68.6092463233164,0.47672495641292));
#18343=CARTESIAN_POINT('Ctrl Pts',(-208.260115679803,66.6049913509854,0.635633275217227));
#18344=CARTESIAN_POINT('Ctrl Pts',(-208.114970174343,63.128085617879,0.794541594021532));
#18345=CARTESIAN_POINT('Ctrl Pts',(-205.113461133577,61.3679192540746,0.95344991282584));
#18346=CARTESIAN_POINT('Ctrl Pts',(-202.00822059199,62.9373177478322,1.11235823163015));
#18347=CARTESIAN_POINT('Ctrl Pts',(-201.645669878913,66.3978992916336,1.27126655043445));
#18348=CARTESIAN_POINT('Ctrl Pts',(-204.358399583502,68.5768348597731,1.43017486923876));
#18349=CARTESIAN_POINT('Ctrl Pts',(-207.659308320785,67.4766010095058,1.58908318804307));
#18350=CARTESIAN_POINT('Ctrl Pts',(-208.522208970686,64.1058310992964,1.74799150684737));
#18351=CARTESIAN_POINT('Ctrl Pts',(-206.155980002522,61.5548329839681,1.90689982565168));
#18352=CARTESIAN_POINT('Ctrl Pts',(-202.729965277546,62.162321722855,2.06580814445599));
#18353=CARTESIAN_POINT('Ctrl Pts',(-201.385091173662,65.3713640166521,2.22471646326029));
#18354=CARTESIAN_POINT('Ctrl Pts',(-203.354325972851,68.2399430433535,2.3836247820646));
#18355=CARTESIAN_POINT('Ctrl Pts',(-206.83229589241,68.1381789310981,2.54253310086891));
#18356=CARTESIAN_POINT('Ctrl Pts',(-208.630437627999,65.1593672402151,2.70144141967321));
#18357=CARTESIAN_POINT('Ctrl Pts',(-207.100234620393,62.0344495464248,2.86034973847752));
#18358=CARTESIAN_POINT('Ctrl Pts',(-203.644560036488,61.6283153137219,3.01925805728183));
#18359=CARTESIAN_POINT('Ctrl Pts',(-201.431537637472,64.3133039407759,3.17816637608613));
#18360=CARTESIAN_POINT('Ctrl Pts',(-202.490041660205,67.6278478282085,3.33707469489044));
#18361=CARTESIAN_POINT('Ctrl Pts',(-205.849647429869,68.5332102033146,3.49598301369475));
#18362=CARTESIAN_POINT('Ctrl Pts',(-208.430305934935,66.1993649512308,3.65489133249905));
#18363=CARTESIAN_POINT('Ctrl Pts',(-207.866098297326,62.7659553182491,3.81379965130336));
#18364=CARTESIAN_POINT('Ctrl Pts',(-204.674283775171,61.380692879392,3.97270797010767));
#18365=CARTESIAN_POINT('Ctrl Pts',(-201.781082247158,63.3135707567762,4.13161628891197));
#18366=CARTESIAN_POINT('Ctrl Pts',(-201.838948537927,66.7925481153239,4.29052460771628));
#18367=CARTESIAN_POINT('Ctrl Pts',(-204.794831478631,68.6281373967567,4.44943292652058));
#18368=CARTESIAN_POINT('Ctrl Pts',(-207.938810626636,67.1374908637484,4.60834124532489));
#18369=CARTESIAN_POINT('Ctrl Pts',(-208.388521038603,63.6872165971666,4.7672495641292));
#18370=CARTESIAN_POINT('Ctrl Pts',(-205.731673235186,61.4404874815853,4.92615788293351));
#18371=CARTESIAN_POINT('Ctrl Pts',(-202.404035587507,62.4570796589551,5.08506620173781));
#18372=CARTESIAN_POINT('Ctrl Pts',(-201.456349098646,65.8049927832981,5.24397452054212));
#18373=CARTESIAN_POINT('Ctrl Pts',(-203.757442149492,68.4148975211522,5.40288283934643));
#18374=CARTESIAN_POINT('Ctrl Pts',(-207.197698349872,67.894062379217,5.56179115815073));
#18375=CARTESIAN_POINT('Ctrl Pts',(-208.623129266309,64.7199831943528,5.72069947695504));
#18376=CARTESIAN_POINT('Ctrl Pts',(-206.726915766361,61.8026202872159,5.87960779575935));
#18377=CARTESIAN_POINT('Ctrl Pts',(-203.247485193193,61.8165793643074,6.03851611456365));
#18378=CARTESIAN_POINT('Ctrl Pts',(-201.374740607411,64.7490628997678,6.19742443336797));
#18379=CARTESIAN_POINT('Ctrl Pts',(-202.825593313979,67.9116027640487,6.35633275217227));
#18380=CARTESIAN_POINT('Ctrl Pts',(-206.269917767397,68.4048177566322,6.51524107097658));
#18381=CARTESIAN_POINT('Ctrl Pts',(-208.549995805274,65.7765338848791,6.67414938978088));
#18382=CARTESIAN_POINT('Ctrl Pts',(-207.575477366445,62.4363324266277,6.83305770858519));
#18383=CARTESIAN_POINT('Ctrl Pts',(-204.239790063637,61.4464727460615,6.99196602738949));
#18384=CARTESIAN_POINT('Ctrl Pts',(-201.601054733778,63.7144471348668,7.1508743461938));
#18385=CARTESIAN_POINT('Ctrl Pts',(-202.078434434683,67.1610020220675,7.3097826649981));
#18386=CARTESIAN_POINT('Ctrl Pts',(-205.234272792136,68.6263744085096,7.46869098380242));
#18387=CARTESIAN_POINT('Ctrl Pts',(-208.175332472178,66.7671272684671,7.62759930260672));
#18388=CARTESIAN_POINT('Ctrl Pts',(-208.205282831762,63.2877975995101,7.78650762141103));
#18389=CARTESIAN_POINT('Ctrl Pts',(-205.29666571597,61.3781959543899,7.94541594021533));
#18390=CARTESIAN_POINT('Ctrl Pts',(-202.116068787548,62.7890237781302,8.10432425901964));
#18391=CARTESIAN_POINT('Ctrl Pts',(-201.579427761599,66.2268498904564,8.26323257782394));
#18392=CARTESIAN_POINT('Ctrl Pts',(-204.178729132788,68.5399137354599,8.42214089662826));
#18393=CARTESIAN_POINT('Ctrl Pts',(-207.530962455862,67.6076242326776,8.58104921543256));
#18394=CARTESIAN_POINT('Ctrl Pts',(-208.562837687446,64.2846939782535,8.73995753423686));
#18395=CARTESIAN_POINT('Ctrl Pts',(-206.328343148279,61.6175482897389,8.89886585304117));
#18396=CARTESIAN_POINT('Ctrl Pts',(-202.876038457388,62.0513965242284,9.05777417184548));
#18397=CARTESIAN_POINT('Ctrl Pts',(-201.370957969684,65.1884914693738,9.21668249064979));
#18398=CARTESIAN_POINT('Ctrl Pts',(-203.192942654321,68.1527795421275,9.37559080945409));
#18399=CARTESIAN_POINT('Ctrl Pts',(-206.671617316371,68.2266345686238,9.5344991282584));
#18400=CARTESIAN_POINT('Ctrl Pts',(-208.617771906093,65.3423470860332,9.69340744706271));
#18401=CARTESIAN_POINT('Ctrl Pts',(-207.247193647397,62.1441996213101,9.85231576586701));
#18402=CARTESIAN_POINT('Ctrl Pts',(-203.816413369187,61.5642180250794,10.0112240846713));
#18403=CARTESIAN_POINT('Ctrl Pts',(-201.470732085403,64.1341229424312,10.1701324034756));
#18404=CARTESIAN_POINT('Ctrl Pts',(-202.360644179824,67.4978542684331,10.3290407222799));
#18405=CARTESIAN_POINT('Ctrl Pts',(-205.670288190648,68.5715807191365,10.4879490410843));
#18406=CARTESIAN_POINT('Ctrl Pts',(-208.365419479959,66.3709218853546,10.6468573598885));
#18407=CARTESIAN_POINT('Ctrl Pts',(-207.975171804641,62.9134171895902,10.8057656786929));
#18408=CARTESIAN_POINT('Ctrl Pts',(-204.857319871709,61.3688682931048,10.9646739974972));
#18409=CARTESIAN_POINT('Ctrl Pts',(-201.870275485688,63.1533003610926,11.1235823163015));
#18410=CARTESIAN_POINT('Ctrl Pts',(-201.752527554104,66.6307660178506,11.2824906351058));
#18411=CARTESIAN_POINT('Ctrl Pts',(-204.61202606459,68.6131636161778,11.4413989539101));
#18412=CARTESIAN_POINT('Ctrl Pts',(-207.827214742755,67.2830531947759,11.6003072727144));
#18413=CARTESIAN_POINT('Ctrl Pts',(-208.450444543957,63.859865121617,11.7592155915187));
#18414=CARTESIAN_POINT('Ctrl Pts',(-205.910345352164,61.4819399619076,11.918123910323));
#18415=CARTESIAN_POINT('Ctrl Pts',(-202.535651716249,62.3293329244922,12.0770322291273));
#18416=CARTESIAN_POINT('Ctrl Pts',(-201.420245043365,65.6251636124073,12.2359405479316));
#18417=CARTESIAN_POINT('Ctrl Pts',(-203.586717704544,68.3478512877946,12.3948488667359));
#18418=CARTESIAN_POINT('Ctrl Pts',(-207.048871778231,68.0012663207677,12.5537571855402));
#18419=CARTESIAN_POINT('Ctrl Pts',(-208.632643105455,64.9031539354061,12.7126655043445));
#18420=CARTESIAN_POINT('Ctrl Pts',(-206.886047834894,61.8938289396112,12.8715738231488));
#18421=CARTESIAN_POINT('Ctrl Pts',(-203.410344989279,61.7322068549995,13.0304821419532));
#18422=CARTESIAN_POINT('Ctrl Pts',(-201.392020090227,64.5664610021721,13.1893904607575));
#18423=CARTESIAN_POINT('Ctrl Pts',(-202.681450846851,67.7981788571913,13.3482987795618));
#18424=CARTESIAN_POINT('Ctrl Pts',(-206.096501553054,68.4645576101642,13.5072070983661));
#18425=CARTESIAN_POINT('Ctrl Pts',(-208.506291890959,65.9546686696882,13.6661154171704));
#18426=CARTESIAN_POINT('Ctrl Pts',(-207.70155301198,62.5695501611123,13.8250237359747));
#18427=CARTESIAN_POINT('Ctrl Pts',(-204.420060527044,61.4126409040308,13.983932054779));
#18428=CARTESIAN_POINT('Ctrl Pts',(-201.670250067554,63.5445823630629,14.1428403735833));
#18429=CARTESIAN_POINT('Ctrl Pts',(-201.973117133283,67.0108344609999,14.3017486923876));
#18430=CARTESIAN_POINT('Ctrl Pts',(-205.050996574037,68.6335759662945,14.4606570111919));
#18431=CARTESIAN_POINT('Ctrl Pts',(-208.082122938738,66.9250957063364,14.6195653299962));
#18432=CARTESIAN_POINT('Ctrl Pts',(-208.287593414598,63.4517090773303,14.7784736488005));
#18433=CARTESIAN_POINT('Ctrl Pts',(-205.479035047994,61.3977785533642,14.9373819676048));
#18434=CARTESIAN_POINT('Ctrl Pts',(-202.231302589651,62.6463237891479,15.0962902864091));
#18435=CARTESIAN_POINT('Ctrl Pts',(-201.521881206253,66.0526943062019,15.2551986052135));
#18436=CARTESIAN_POINT('Ctrl Pts',(-204.001159776429,68.4939639011247,15.4141069240177));
#18437=CARTESIAN_POINT('Ctrl Pts',(-207.396164892643,67.7320116880119,15.5730152428221));
#18438=CARTESIAN_POINT('Ctrl Pts',(-208.594390772745,64.4653708967053,15.7319235616264));
#18439=CARTESIAN_POINT('Ctrl Pts',(-206.497323573879,61.6888943200732,15.8908318804307));
#18440=CARTESIAN_POINT('Ctrl Pts',(-203.027518195758,61.9479566643454,16.049740199235));
#18441=CARTESIAN_POINT('Ctrl Pts',(-201.366079921308,65.0051924257885,16.2086485180393));
#18442=CARTESIAN_POINT('Ctrl Pts',(-203.036142251593,68.0574739112173,16.3675568368436));
#18443=CARTESIAN_POINT('Ctrl Pts',(-206.506722984033,68.3070966859805,16.5264651556479));
#18444=CARTESIAN_POINT('Ctrl Pts',(-208.595801399242,65.5239883392264,16.6853734744522));
#18445=CARTESIAN_POINT('Ctrl Pts',(-207.388609787001,62.2621850922406,16.8442817932565));
#18446=CARTESIAN_POINT('Ctrl Pts',(-203.990917570668,61.5068826602371,17.0031901120608));
#18447=CARTESIAN_POINT('Ctrl Pts',(-201.519757996531,63.9612260827295,17.1620984308651));
#18448=CARTESIAN_POINT('Ctrl Pts',(-201.999201820237,66.219820647773,17.268037310068));
#18449=CARTESIAN_POINT('Ctrl Pts',(-202.663937342304,66.9973015569306,17.3210067496694));
#18450=CARTESIAN_POINT('Ctrl Pts',(-204.254067145653,62.2098224301579,-0.107002249889811));
#18451=CARTESIAN_POINT('Ctrl Pts',(-203.325449162499,62.4580814192126,-0.0540328102883756));
#18452=CARTESIAN_POINT('Ctrl Pts',(-201.75194824434,63.9519550145908,0.0519060689144955));
#18453=CARTESIAN_POINT('Ctrl Pts',(-202.359224806561,67.1679796199166,0.210814387718803));
#18454=CARTESIAN_POINT('Ctrl Pts',(-205.392461749333,68.3916072629874,0.369722706523109));
#18455=CARTESIAN_POINT('Ctrl Pts',(-208.063529343057,66.5082097023603,0.528631025327416));
#18456=CARTESIAN_POINT('Ctrl Pts',(-207.927136172181,63.2409628367347,0.687539344131722));
#18457=CARTESIAN_POINT('Ctrl Pts',(-205.106619379847,61.5869352396215,0.846447662936029));
#18458=CARTESIAN_POINT('Ctrl Pts',(-202.188626139504,63.0616983489064,1.00535598174034));
#18459=CARTESIAN_POINT('Ctrl Pts',(-201.847937385808,66.3136053806583,1.16426430054464));
#18460=CARTESIAN_POINT('Ctrl Pts',(-204.397088356516,68.3611502242289,1.32317261934895));
#18461=CARTESIAN_POINT('Ctrl Pts',(-207.498950918653,67.3272609345331,1.48208093815326));
#18462=CARTESIAN_POINT('Ctrl Pts',(-208.309818299063,64.1597498573671,1.64098925695756));
#18463=CARTESIAN_POINT('Ctrl Pts',(-206.086273925693,61.7625779935569,1.79989757576187));
#18464=CARTESIAN_POINT('Ctrl Pts',(-202.866849319158,62.3334349078333,1.95880589456617));
#18465=CARTESIAN_POINT('Ctrl Pts',(-201.603071685287,65.3489706113857,2.11771421337048));
#18466=CARTESIAN_POINT('Ctrl Pts',(-203.453560803836,68.0445731250081,2.27662253217479));
#18467=CARTESIAN_POINT('Ctrl Pts',(-206.721807685027,67.9489454312129,2.4355308509791));
#18468=CARTESIAN_POINT('Ctrl Pts',(-208.41152072315,65.1497573290867,2.5944391697834));
#18469=CARTESIAN_POINT('Ctrl Pts',(-206.973589595835,62.2132734770346,2.75334748858771));
#18470=CARTESIAN_POINT('Ctrl Pts',(-203.726293632249,61.8316293081442,2.91225580739202));
#18471=CARTESIAN_POINT('Ctrl Pts',(-201.646717407937,64.3547119998756,3.07116412619632));
#18472=CARTESIAN_POINT('Ctrl Pts',(-202.641393196122,67.4693875069152,3.23007244500063));
#18473=CARTESIAN_POINT('Ctrl Pts',(-205.79841333508,68.3201561527704,3.38898076380493));
#18474=CARTESIAN_POINT('Ctrl Pts',(-208.223457054742,66.1270427438794,3.54788908260924));
#18475=CARTESIAN_POINT('Ctrl Pts',(-207.693271373264,62.9006691453792,3.70679740141355));
#18476=CARTESIAN_POINT('Ctrl Pts',(-204.69392459953,61.5989386099986,3.86570572021786));
#18477=CARTESIAN_POINT('Ctrl Pts',(-201.975184331707,63.4152631443075,4.02461403902216));
#18478=CARTESIAN_POINT('Ctrl Pts',(-202.02956126098,66.6844567154952,4.18352235782647));
#18479=CARTESIAN_POINT('Ctrl Pts',(-204.807203226137,68.4093591968113,4.34243067663077));
#18480=CARTESIAN_POINT('Ctrl Pts',(-207.761599118756,67.0085992721596,4.50133899543508));
#18481=CARTESIAN_POINT('Ctrl Pts',(-208.184191805105,63.7663779845074,4.66024731423939));
#18482=CARTESIAN_POINT('Ctrl Pts',(-205.687553033595,61.6551275727124,4.8191556330437));
#18483=CARTESIAN_POINT('Ctrl Pts',(-202.56057332552,62.6104188173111,4.97806395184801));
#18484=CARTESIAN_POINT('Ctrl Pts',(-201.670032727642,65.7564513823422,5.13697227065231));
#18485=CARTESIAN_POINT('Ctrl Pts',(-203.832368906705,68.2089777747436,5.29588058945662));
#18486=CARTESIAN_POINT('Ctrl Pts',(-207.06517622173,67.7195492093407,5.45478890826092));
#18487=CARTESIAN_POINT('Ctrl Pts',(-208.404653058721,64.7368683246537,5.61369722706523));
#18488=CARTESIAN_POINT('Ctrl Pts',(-206.622782024579,61.9954236189558,5.77260554586954));
#18489=CARTESIAN_POINT('Ctrl Pts',(-203.353162567803,62.0085409578702,5.93151386467384));
#18490=CARTESIAN_POINT('Ctrl Pts',(-201.593345262503,64.76419451169,6.09042218347815));
#18491=CARTESIAN_POINT('Ctrl Pts',(-202.956710945065,67.7360319016432,6.24933050228246));
#18492=CARTESIAN_POINT('Ctrl Pts',(-206.193341195772,68.1995058242328,6.40823882108676));
#18493=CARTESIAN_POINT('Ctrl Pts',(-208.335929575923,65.729708567381,6.56714713989107));
#18494=CARTESIAN_POINT('Ctrl Pts',(-207.420175005863,62.5909226517559,6.72605545869538));
#18495=CARTESIAN_POINT('Ctrl Pts',(-204.285631040223,61.6607519232417,6.88496377749968));
#18496=CARTESIAN_POINT('Ctrl Pts',(-201.806012552553,63.7919665094142,7.04387209630399));
#18497=CARTESIAN_POINT('Ctrl Pts',(-202.254606058165,67.0306926978151,7.2027804151083));
#18498=CARTESIAN_POINT('Ctrl Pts',(-205.22014604495,68.4077025174916,7.3616887339126));
#18499=CARTESIAN_POINT('Ctrl Pts',(-207.983858598253,66.6605687563183,7.52059705271691));
#18500=CARTESIAN_POINT('Ctrl Pts',(-208.012002938647,63.391044119186,7.67950537152122));
#18501=CARTESIAN_POINT('Ctrl Pts',(-205.278776649425,61.5965922506168,7.83841369032552));
#18502=CARTESIAN_POINT('Ctrl Pts',(-202.289971043838,62.9223465674972,7.99732200912984));
#18503=CARTESIAN_POINT('Ctrl Pts',(-201.785689695828,66.1528703297934,8.15623032793413));
#18504=CARTESIAN_POINT('Ctrl Pts',(-204.228252109001,68.3264554591282,8.31513864673845));
#18505=CARTESIAN_POINT('Ctrl Pts',(-207.378344362975,67.4503834026392,8.47404696554275));
#18506=CARTESIAN_POINT('Ctrl Pts',(-208.347997087237,64.3278272300392,8.63295528434705));
#18507=CARTESIAN_POINT('Ctrl Pts',(-206.248243501792,61.8215115402032,8.79186360315136));
#18508=CARTESIAN_POINT('Ctrl Pts',(-203.004114225263,62.2291985450005,8.95077192195567));
#18509=CARTESIAN_POINT('Ctrl Pts',(-201.589790719411,65.1771253550663,9.10968024075998));
#18510=CARTESIAN_POINT('Ctrl Pts',(-203.301908966799,67.9626656193009,9.26858855956429));
#18511=CARTESIAN_POINT('Ctrl Pts',(-206.570818094213,68.0320671568614,9.42749687836859));
#18512=CARTESIAN_POINT('Ctrl Pts',(-208.399618749562,65.3217034137992,9.58640519717289));
#18513=CARTESIAN_POINT('Ctrl Pts',(-207.111686932148,62.3164055765784,9.7453135159772));
#18514=CARTESIAN_POINT('Ctrl Pts',(-203.887784137229,61.7713971127705,9.90422183478151));
#18515=CARTESIAN_POINT('Ctrl Pts',(-201.683548414291,64.1863356905477,10.0631301535858));
#18516=CARTESIAN_POINT('Ctrl Pts',(-202.519798437837,67.347232613073,10.2220384723901));
#18517=CARTESIAN_POINT('Ctrl Pts',(-205.629869532874,68.3562129104667,10.3809467911944));
#18518=CARTESIAN_POINT('Ctrl Pts',(-208.162483280093,66.2882547232422,10.5398551099987));
#18519=CARTESIAN_POINT('Ctrl Pts',(-207.795767702545,63.0392390043061,10.698763428803));
#18520=CARTESIAN_POINT('Ctrl Pts',(-204.86592354302,61.5878270512018,10.8576717476073));
#18521=CARTESIAN_POINT('Ctrl Pts',(-202.05899918071,63.2646571204042,11.0165800664117));
#18522=CARTESIAN_POINT('Ctrl Pts',(-201.948351498567,66.5324301460514,11.175488385216));
#18523=CARTESIAN_POINT('Ctrl Pts',(-204.635421054893,68.3952883414536,11.3343967040203));
#18524=CARTESIAN_POINT('Ctrl Pts',(-207.65673251327,67.145384133847,11.4933050228246));
#18525=CARTESIAN_POINT('Ctrl Pts',(-208.242381297231,63.9286157308444,11.6522133416289));
#18526=CARTESIAN_POINT('Ctrl Pts',(-205.855451147316,61.694080451163,11.8111216604332));
#18527=CARTESIAN_POINT('Ctrl Pts',(-202.684252946743,62.4903752642767,11.9700299792375));
#18528=CARTESIAN_POINT('Ctrl Pts',(-201.636105761969,65.5874659855433,12.1289382980418));
#18529=CARTESIAN_POINT('Ctrl Pts',(-203.671939217073,68.1459744572525,12.2878466168461));
#18530=CARTESIAN_POINT('Ctrl Pts',(-206.925323954502,67.8202887084531,12.4467549356504));
#18531=CARTESIAN_POINT('Ctrl Pts',(-208.413593209394,64.9089937935389,12.6056632544547));
#18532=CARTESIAN_POINT('Ctrl Pts',(-206.772318362935,62.0811323515277,12.764571573259));
#18533=CARTESIAN_POINT('Ctrl Pts',(-203.506201850182,61.929256146103,12.9234798920633));
#18534=CARTESIAN_POINT('Ctrl Pts',(-201.609582785291,64.5926035847644,13.0823882108676));
#18535=CARTESIAN_POINT('Ctrl Pts',(-202.821260328891,67.6294475037291,13.241296529672));
#18536=CARTESIAN_POINT('Ctrl Pts',(-206.030382051563,68.2556433396526,13.4002048484763));
#18537=CARTESIAN_POINT('Ctrl Pts',(-208.29486102589,65.8971017502862,13.5591131672806));
#18538=CARTESIAN_POINT('Ctrl Pts',(-207.53864823733,62.7161073012263,13.7180214860849));
#18539=CARTESIAN_POINT('Ctrl Pts',(-204.455031119415,61.6289601554119,13.8769298048892));
#18540=CARTESIAN_POINT('Ctrl Pts',(-201.871035378811,63.6323446542768,14.0358381236935));
#18541=CARTESIAN_POINT('Ctrl Pts',(-202.155639434015,66.889580303382,14.1947464424978));
#18542=CARTESIAN_POINT('Ctrl Pts',(-205.047921459329,68.4144698183351,14.3536547613021));
#18543=CARTESIAN_POINT('Ctrl Pts',(-207.896269638598,66.8090116314247,14.5125630801064));
#18544=CARTESIAN_POINT('Ctrl Pts',(-208.089350158971,63.5450716664528,14.6714713989107));
#18545=CARTESIAN_POINT('Ctrl Pts',(-205.45014903458,61.6149940106962,14.830379717715));
#18546=CARTESIAN_POINT('Ctrl Pts',(-202.398256199559,62.7882514474348,14.9892880365193));
#18547=CARTESIAN_POINT('Ctrl Pts',(-201.731613221797,65.9892163999876,15.1481963553236));
#18548=CARTESIAN_POINT('Ctrl Pts',(-204.061390258974,68.2832764189897,15.3071046741279));
#18549=CARTESIAN_POINT('Ctrl Pts',(-207.251675149103,67.5672702424791,15.4660129929322));
#18550=CARTESIAN_POINT('Ctrl Pts',(-208.377647508318,64.4976092548672,15.6249213117366));
#18551=CARTESIAN_POINT('Ctrl Pts',(-206.40703433717,61.8885553751179,15.7838296305409));
#18552=CARTESIAN_POINT('Ctrl Pts',(-203.146459672159,62.1319961518595,15.9427379493452));
#18553=CARTESIAN_POINT('Ctrl Pts',(-201.585206819389,65.0048793203454,16.1016462681495));
#18554=CARTESIAN_POINT('Ctrl Pts',(-203.154563693826,67.8731069577291,16.2605545869538));
#18555=CARTESIAN_POINT('Ctrl Pts',(-206.415866958967,68.1076773749448,16.4194629057581));
#18556=CARTESIAN_POINT('Ctrl Pts',(-208.378973073449,65.4923916235809,16.5783712245624));
#18557=CARTESIAN_POINT('Ctrl Pts',(-207.244575619486,62.4272764743473,16.7372795433667));
#18558=CARTESIAN_POINT('Ctrl Pts',(-204.051765662497,61.7175190943685,16.896187862171));
#18559=CARTESIAN_POINT('Ctrl Pts',(-201.729618042508,64.0238645836787,17.0550961809753));
#18560=CARTESIAN_POINT('Ctrl Pts',(-202.180151203454,66.1462649533788,17.1610350601782));
#18561=CARTESIAN_POINT('Ctrl Pts',(-202.804802895981,66.8768634390786,17.2140044997796));
#18562=CARTESIAN_POINT('Ctrl Pts',(-204.301933573839,62.3888678140614,-0.214004499779622));
#18563=CARTESIAN_POINT('Ctrl Pts',(-203.43290490324,62.6211960514381,-0.161035060178186));
#18564=CARTESIAN_POINT('Ctrl Pts',(-201.960375363752,64.0192079445796,-0.0550961809753149));
#18565=CARTESIAN_POINT('Ctrl Pts',(-202.52868305661,67.0288606091631,0.103812137828991));
#18566=CARTESIAN_POINT('Ctrl Pts',(-205.367277522588,68.1739682026583,0.262720456633299));
#18567=CARTESIAN_POINT('Ctrl Pts',(-207.86694300631,66.4114280537352,0.421628775437604));
#18568=CARTESIAN_POINT('Ctrl Pts',(-207.739302170019,63.3538400555904,0.580537094241912));
#18569=CARTESIAN_POINT('Ctrl Pts',(-205.099777626116,61.8059512251683,0.739445413046217));
#18570=CARTESIAN_POINT('Ctrl Pts',(-202.369031687018,63.1860789499808,0.898353731850525));
#18571=CARTESIAN_POINT('Ctrl Pts',(-202.050204892703,66.229311469683,1.05726205065483));
#18572=CARTESIAN_POINT('Ctrl Pts',(-204.43577712953,68.1454655886849,1.21617036945914));
#18573=CARTESIAN_POINT('Ctrl Pts',(-207.338593516521,67.1779208595605,1.37507868826344));
#18574=CARTESIAN_POINT('Ctrl Pts',(-208.09742762744,64.2136686154378,1.53398700706775));
#18575=CARTESIAN_POINT('Ctrl Pts',(-206.016567848864,61.9703230031457,1.69289532587206));
#18576=CARTESIAN_POINT('Ctrl Pts',(-203.00373336077,62.5045480928116,1.85180364467637));
#18577=CARTESIAN_POINT('Ctrl Pts',(-201.821052196913,65.3265772061194,2.01071196348067));
#18578=CARTESIAN_POINT('Ctrl Pts',(-203.55279563482,67.8492032066626,2.16962028228498));
#18579=CARTESIAN_POINT('Ctrl Pts',(-206.611319477643,67.7597119313279,2.32852860108929));
#18580=CARTESIAN_POINT('Ctrl Pts',(-208.1926038183,65.1401474179583,2.48743691989359));
#18581=CARTESIAN_POINT('Ctrl Pts',(-206.846944571277,62.3920974076444,2.6463452386979));
#18582=CARTESIAN_POINT('Ctrl Pts',(-203.80802722801,62.0349433025665,2.80525355750221));
#18583=CARTESIAN_POINT('Ctrl Pts',(-201.861897178401,64.3961200589753,2.96416187630651));
#18584=CARTESIAN_POINT('Ctrl Pts',(-202.79274473204,67.310927185622,3.12307019511082));
#18585=CARTESIAN_POINT('Ctrl Pts',(-205.74717924029,68.1071021022261,3.28197851391513));
#18586=CARTESIAN_POINT('Ctrl Pts',(-208.016608174548,66.0547205365278,3.44088683271943));
#18587=CARTESIAN_POINT('Ctrl Pts',(-207.520444449202,63.0353829725094,3.59979515152374));
#18588=CARTESIAN_POINT('Ctrl Pts',(-204.713565423889,61.8171843406052,3.75870347032804));
#18589=CARTESIAN_POINT('Ctrl Pts',(-202.169286416255,63.5169555318388,3.91761178913235));
#18590=CARTESIAN_POINT('Ctrl Pts',(-202.220173984034,66.5763653156666,4.07652010793666));
#18591=CARTESIAN_POINT('Ctrl Pts',(-204.819574973643,68.1905809968658,4.23542842674096));
#18592=CARTESIAN_POINT('Ctrl Pts',(-207.584387610876,66.8797076805709,4.39433674554527));
#18593=CARTESIAN_POINT('Ctrl Pts',(-207.979862571607,63.8455393718481,4.55324506434958));
#18594=CARTESIAN_POINT('Ctrl Pts',(-205.643432832005,61.8697676638397,4.71215338315388));
#18595=CARTESIAN_POINT('Ctrl Pts',(-202.717111063532,62.7637579756671,4.87106170195819));
#18596=CARTESIAN_POINT('Ctrl Pts',(-201.883716356637,65.7079099813863,5.0299700207625));
#18597=CARTESIAN_POINT('Ctrl Pts',(-203.907295663918,68.003058028335,5.18887833956681));
#18598=CARTESIAN_POINT('Ctrl Pts',(-206.932654093589,67.5450360394643,5.34778665837111));
#18599=CARTESIAN_POINT('Ctrl Pts',(-208.186176851132,64.7537534549547,5.50669497717542));
#18600=CARTESIAN_POINT('Ctrl Pts',(-206.518648282798,62.1882269506957,5.66560329597972));
#18601=CARTESIAN_POINT('Ctrl Pts',(-203.458839942412,62.200502551433,5.82451161478403));
#18602=CARTESIAN_POINT('Ctrl Pts',(-201.811949917596,64.7793261236122,5.98341993358834));
#18603=CARTESIAN_POINT('Ctrl Pts',(-203.087828576151,67.5604610392376,6.14232825239265));
#18604=CARTESIAN_POINT('Ctrl Pts',(-206.116764624146,67.9941938918335,6.30123657119695));
#18605=CARTESIAN_POINT('Ctrl Pts',(-208.121863346572,65.6828832498826,6.46014489000126));
#18606=CARTESIAN_POINT('Ctrl Pts',(-207.264872645281,62.7455128768842,6.61905320880557));
#18607=CARTESIAN_POINT('Ctrl Pts',(-204.33147201681,61.8750311004219,6.77796152760987));
#18608=CARTESIAN_POINT('Ctrl Pts',(-202.010970371329,63.8694858839615,6.93686984641418));
#18609=CARTESIAN_POINT('Ctrl Pts',(-202.430777681647,66.9003833735627,7.09577816521848));
#18610=CARTESIAN_POINT('Ctrl Pts',(-205.206019297764,68.1890306264736,7.25468648402279));
#18611=CARTESIAN_POINT('Ctrl Pts',(-207.792384724327,66.5540102441695,7.4135948028271));
#18612=CARTESIAN_POINT('Ctrl Pts',(-207.818723045533,63.494290638862,7.57250312163141));
#18613=CARTESIAN_POINT('Ctrl Pts',(-205.260887582879,61.8149885468436,7.73141144043571));
#18614=CARTESIAN_POINT('Ctrl Pts',(-202.463873300128,63.0556693568644,7.89031975924003));
#18615=CARTESIAN_POINT('Ctrl Pts',(-201.991951630056,66.0788907691303,8.04922807804431));
#18616=CARTESIAN_POINT('Ctrl Pts',(-204.277775085214,68.1129971827966,8.20813639684864));
#18617=CARTESIAN_POINT('Ctrl Pts',(-207.225726270089,67.2931425726009,8.36704471565293));
#18618=CARTESIAN_POINT('Ctrl Pts',(-208.133156487029,64.370960481825,8.52595303445724));
#18619=CARTESIAN_POINT('Ctrl Pts',(-206.168143855303,62.0254747906674,8.68486135326155));
#18620=CARTESIAN_POINT('Ctrl Pts',(-203.132189993138,62.4070005657726,8.84376967206587));
#18621=CARTESIAN_POINT('Ctrl Pts',(-201.808623469137,65.1657592407589,9.00267799087016));
#18622=CARTESIAN_POINT('Ctrl Pts',(-203.410875279276,67.7725516964743,9.16158630967448));
#18623=CARTESIAN_POINT('Ctrl Pts',(-206.470018872056,67.8374997450991,9.32049462847877));
#18624=CARTESIAN_POINT('Ctrl Pts',(-208.181465593032,65.301059741565,9.47940294728309));
#18625=CARTESIAN_POINT('Ctrl Pts',(-206.9761802169,62.4886115318467,9.63831126608739));
#18626=CARTESIAN_POINT('Ctrl Pts',(-203.959154905271,61.9785762004616,9.7972195848917));
#18627=CARTESIAN_POINT('Ctrl Pts',(-201.89636474318,64.2385484386642,9.95612790369601));
#18628=CARTESIAN_POINT('Ctrl Pts',(-202.678952695852,67.1966109577127,10.1150362225003));
#18629=CARTESIAN_POINT('Ctrl Pts',(-205.589450875101,68.1408451017969,10.2739445413046));
#18630=CARTESIAN_POINT('Ctrl Pts',(-207.959547080228,66.2055875611298,10.4328528601089));
#18631=CARTESIAN_POINT('Ctrl Pts',(-207.616363600448,63.165060819022,10.5917611789132));
#18632=CARTESIAN_POINT('Ctrl Pts',(-204.874527214332,61.8067858092989,10.7506694977175));
#18633=CARTESIAN_POINT('Ctrl Pts',(-202.247722875733,63.3760138797158,10.9095778165218));
#18634=CARTESIAN_POINT('Ctrl Pts',(-202.144175443029,66.4340942742521,11.0684861353262));
#18635=CARTESIAN_POINT('Ctrl Pts',(-204.658816045196,68.1774130667293,11.2273944541305));
#18636=CARTESIAN_POINT('Ctrl Pts',(-207.486250283784,67.007715072918,11.3863027729348));
#18637=CARTESIAN_POINT('Ctrl Pts',(-208.034318050505,63.9973663400718,11.5452110917391));
#18638=CARTESIAN_POINT('Ctrl Pts',(-205.800556942468,61.9062209404184,11.7041194105434));
#18639=CARTESIAN_POINT('Ctrl Pts',(-202.832854177236,62.6514176040611,11.8630277293477));
#18640=CARTESIAN_POINT('Ctrl Pts',(-201.851966480573,65.5497683586795,12.021936048152));
#18641=CARTESIAN_POINT('Ctrl Pts',(-203.757160729602,67.9440976267103,12.1808443669563));
#18642=CARTESIAN_POINT('Ctrl Pts',(-206.801776130772,67.6393110961385,12.3397526857606));
#18643=CARTESIAN_POINT('Ctrl Pts',(-208.194543313332,64.9148336516718,12.4986610045649));
#18644=CARTESIAN_POINT('Ctrl Pts',(-206.658588890975,62.2684357634442,12.6575693233692));
#18645=CARTESIAN_POINT('Ctrl Pts',(-203.602058711086,62.1263054372066,12.8164776421735));
#18646=CARTESIAN_POINT('Ctrl Pts',(-201.827145480354,64.6187461673567,12.9753859609778));
#18647=CARTESIAN_POINT('Ctrl Pts',(-202.961069810931,67.4607161502669,13.1342942797821));
#18648=CARTESIAN_POINT('Ctrl Pts',(-205.964262550072,68.0467290691411,13.2932025985864));
#18649=CARTESIAN_POINT('Ctrl Pts',(-208.08343016082,65.8395348308842,13.4521109173908));
#18650=CARTESIAN_POINT('Ctrl Pts',(-207.37574346268,62.8626644413404,13.611019236195));
#18651=CARTESIAN_POINT('Ctrl Pts',(-204.490001711787,61.8452794067929,13.7699275549994));
#18652=CARTESIAN_POINT('Ctrl Pts',(-202.071820690067,63.7201069454906,13.9288358738037));
#18653=CARTESIAN_POINT('Ctrl Pts',(-202.338161734746,66.768326145764,14.087744192608));
#18654=CARTESIAN_POINT('Ctrl Pts',(-205.044846344621,68.1953636703757,14.2466525114123));
#18655=CARTESIAN_POINT('Ctrl Pts',(-207.710416338458,66.692927556513,14.4055608302166));
#18656=CARTESIAN_POINT('Ctrl Pts',(-207.891106903343,63.6384342555754,14.5644691490209));
#18657=CARTESIAN_POINT('Ctrl Pts',(-205.421263021166,61.8322094680282,14.7233774678252));
#18658=CARTESIAN_POINT('Ctrl Pts',(-202.565209809467,62.9301791057216,14.8822857866295));
#18659=CARTESIAN_POINT('Ctrl Pts',(-201.941345237341,65.9257384937735,15.0411941054338));
#18660=CARTESIAN_POINT('Ctrl Pts',(-204.121620741519,68.0725889368547,15.2001024242381));
#18661=CARTESIAN_POINT('Ctrl Pts',(-207.107185405563,67.4025287969464,15.3590107430424));
#18662=CARTESIAN_POINT('Ctrl Pts',(-208.160904243891,64.5298476130291,15.5179190618467));
#18663=CARTESIAN_POINT('Ctrl Pts',(-206.316745100461,62.0882164301626,15.676827380651));
#18664=CARTESIAN_POINT('Ctrl Pts',(-203.26540114856,62.3160356393736,15.8357356994554));
#18665=CARTESIAN_POINT('Ctrl Pts',(-201.80433371747,65.0045662149023,15.9946440182597));
#18666=CARTESIAN_POINT('Ctrl Pts',(-203.27298513606,67.6887400042411,16.153552337064));
#18667=CARTESIAN_POINT('Ctrl Pts',(-206.325010933901,67.908258063909,16.3124606558683));
#18668=CARTESIAN_POINT('Ctrl Pts',(-208.162144747655,65.4607949079353,16.4713689746726));
#18669=CARTESIAN_POINT('Ctrl Pts',(-207.100541451971,62.5923678564539,16.6302772934769));
#18670=CARTESIAN_POINT('Ctrl Pts',(-204.112613754326,61.9281555284998,16.7891856122812));
#18671=CARTESIAN_POINT('Ctrl Pts',(-201.939478088485,64.086503084628,16.9480939310855));
#18672=CARTESIAN_POINT('Ctrl Pts',(-202.36110058667,66.0727092589846,17.0540328102884));
#18673=CARTESIAN_POINT('Ctrl Pts',(-202.945668449658,66.7564253212267,17.1070022498898));
#18674=CARTESIAN_POINT('Ctrl Pts',(-204.349800002025,62.567913197965,-0.321006749669432));
#18675=CARTESIAN_POINT('Ctrl Pts',(-203.540360643981,62.7843106836636,-0.268037310067997));
#18676=CARTESIAN_POINT('Ctrl Pts',(-202.168802483164,64.0864608745682,-0.162098430865125));
#18677=CARTESIAN_POINT('Ctrl Pts',(-202.69814130666,66.8897415984097,-0.00319011206081897));
#18678=CARTESIAN_POINT('Ctrl Pts',(-205.342093295844,67.9563291423292,0.155718206743488));
#18679=CARTESIAN_POINT('Ctrl Pts',(-207.670356669564,66.3146464051101,0.314626525547794));
#18680=CARTESIAN_POINT('Ctrl Pts',(-207.551468167857,63.4667172744462,0.4735348443521));
#18681=CARTESIAN_POINT('Ctrl Pts',(-205.092935872386,62.0249672107152,0.632443163156408));
#18682=CARTESIAN_POINT('Ctrl Pts',(-202.549437234532,63.310459551055,0.791351481960714));
#18683=CARTESIAN_POINT('Ctrl Pts',(-202.252472399597,66.1450175587076,0.950259800765021));
#18684=CARTESIAN_POINT('Ctrl Pts',(-204.474465902543,67.9297809531409,1.10916811956933));
#18685=CARTESIAN_POINT('Ctrl Pts',(-207.178236114389,67.0285807845878,1.26807643837363));
#18686=CARTESIAN_POINT('Ctrl Pts',(-207.885036955817,64.2675873735086,1.42698475717794));
#18687=CARTESIAN_POINT('Ctrl Pts',(-205.946861772035,62.1780680127346,1.58589307598225));
#18688=CARTESIAN_POINT('Ctrl Pts',(-203.140617402382,62.67566127779,1.74480139478655));
#18689=CARTESIAN_POINT('Ctrl Pts',(-202.039032708539,65.304183800853,1.90370971359086));
#18690=CARTESIAN_POINT('Ctrl Pts',(-203.652030465805,67.6538332883171,2.06261803239516));
#18691=CARTESIAN_POINT('Ctrl Pts',(-206.50083127026,67.5704784314428,2.22152635119948));
#18692=CARTESIAN_POINT('Ctrl Pts',(-207.97368691345,65.1305375068299,2.38043467000378));
#18693=CARTESIAN_POINT('Ctrl Pts',(-206.720299546718,62.5709213382542,2.53934298880809));
#18694=CARTESIAN_POINT('Ctrl Pts',(-203.88976082377,62.2382572969888,2.6982513076124));
#18695=CARTESIAN_POINT('Ctrl Pts',(-202.077076948865,64.4375281180749,2.8571596264167));
#18696=CARTESIAN_POINT('Ctrl Pts',(-202.944096267957,67.1524668643289,3.01606794522101));
#18697=CARTESIAN_POINT('Ctrl Pts',(-205.6959451455,67.8940480516819,3.17497626402531));
#18698=CARTESIAN_POINT('Ctrl Pts',(-207.809759294355,65.9823983291764,3.33388458282962));
#18699=CARTESIAN_POINT('Ctrl Pts',(-207.34761752514,63.1700967996395,3.49279290163393));
#18700=CARTESIAN_POINT('Ctrl Pts',(-204.733206248249,62.0354300712118,3.65170122043824));
#18701=CARTESIAN_POINT('Ctrl Pts',(-202.363388500804,63.6186479193701,3.81060953924254));
#18702=CARTESIAN_POINT('Ctrl Pts',(-202.410786707087,66.4682739158379,3.96951785804685));
#18703=CARTESIAN_POINT('Ctrl Pts',(-204.831946721149,67.9718027969204,4.12842617685115));
#18704=CARTESIAN_POINT('Ctrl Pts',(-207.407176102995,66.7508160889821,4.28733449565546));
#18705=CARTESIAN_POINT('Ctrl Pts',(-207.77553333811,63.9247007591889,4.44624281445977));
#18706=CARTESIAN_POINT('Ctrl Pts',(-205.599312630415,62.0844077549669,4.60515113326408));
#18707=CARTESIAN_POINT('Ctrl Pts',(-202.873648801545,62.9170971340231,4.76405945206838));
#18708=CARTESIAN_POINT('Ctrl Pts',(-202.097399985633,65.6593685804304,4.92296777087269));
#18709=CARTESIAN_POINT('Ctrl Pts',(-203.982222421131,67.7971382819264,5.08187608967699));
#18710=CARTESIAN_POINT('Ctrl Pts',(-206.800131965447,67.370522869588,5.2407844084813));
#18711=CARTESIAN_POINT('Ctrl Pts',(-207.967700643544,64.7706385852557,5.39969272728561));
#18712=CARTESIAN_POINT('Ctrl Pts',(-206.414514541016,62.3810302824357,5.55860104608992));
#18713=CARTESIAN_POINT('Ctrl Pts',(-203.564517317021,62.3924641449957,5.71750936489422));
#18714=CARTESIAN_POINT('Ctrl Pts',(-202.030554572688,64.7944577355345,5.87641768369853));
#18715=CARTESIAN_POINT('Ctrl Pts',(-203.218946207237,67.3848901768319,6.03532600250283));
#18716=CARTESIAN_POINT('Ctrl Pts',(-206.040188052521,67.7888819594342,6.19423432130714));
#18717=CARTESIAN_POINT('Ctrl Pts',(-207.907797117221,65.6360579323843,6.35314264011145));
#18718=CARTESIAN_POINT('Ctrl Pts',(-207.1095702847,62.9001031020125,6.51205095891576));
#18719=CARTESIAN_POINT('Ctrl Pts',(-204.377312993397,62.089310277602,6.67095927772006));
#18720=CARTESIAN_POINT('Ctrl Pts',(-202.215928190104,63.9470052585089,6.82986759652437));
#18721=CARTESIAN_POINT('Ctrl Pts',(-202.606949305129,66.7700740493103,6.98877591532868));
#18722=CARTESIAN_POINT('Ctrl Pts',(-205.191892550579,67.9703587354556,7.14768423413298));
#18723=CARTESIAN_POINT('Ctrl Pts',(-207.600910850401,66.4474517320208,7.30659255293729));
#18724=CARTESIAN_POINT('Ctrl Pts',(-207.625443152419,63.597537158538,7.4655008717416));
#18725=CARTESIAN_POINT('Ctrl Pts',(-205.242998516334,62.0333848430704,7.6244091905459));
#18726=CARTESIAN_POINT('Ctrl Pts',(-202.637775556419,63.1889921462316,7.78331750935021));
#18727=CARTESIAN_POINT('Ctrl Pts',(-202.198213564284,66.0049112084673,7.94222582815451));
#18728=CARTESIAN_POINT('Ctrl Pts',(-204.327298061427,67.8995389064651,8.10113414695883));
#18729=CARTESIAN_POINT('Ctrl Pts',(-207.073108177202,67.1359017425625,8.26004246576313));
#18730=CARTESIAN_POINT('Ctrl Pts',(-207.918315886821,64.4140937336109,8.41895078456743));
#18731=CARTESIAN_POINT('Ctrl Pts',(-206.088044208815,62.2294380411316,8.57785910337174));
#18732=CARTESIAN_POINT('Ctrl Pts',(-203.260265761013,62.5848025865447,8.73676742217605));
#18733=CARTESIAN_POINT('Ctrl Pts',(-202.027456218864,65.1543931264515,8.89567574098036));
#18734=CARTESIAN_POINT('Ctrl Pts',(-203.519841591753,67.5824377736476,9.05458405978466));
#18735=CARTESIAN_POINT('Ctrl Pts',(-206.369219649899,67.6429323333367,9.21349237858897));
#18736=CARTESIAN_POINT('Ctrl Pts',(-207.963312436502,65.2804160693309,9.37240069739327));
#18737=CARTESIAN_POINT('Ctrl Pts',(-206.840673501651,62.6608174871151,9.53130901619759));
#18738=CARTESIAN_POINT('Ctrl Pts',(-204.030525673313,62.1857552881527,9.69021733500189));
#18739=CARTESIAN_POINT('Ctrl Pts',(-202.109181072068,64.2907611867807,9.8491256538062));
#18740=CARTESIAN_POINT('Ctrl Pts',(-202.838106953866,67.0459893023525,10.0080339726105));
#18741=CARTESIAN_POINT('Ctrl Pts',(-205.549032217327,67.925477293127,10.1669422914148));
#18742=CARTESIAN_POINT('Ctrl Pts',(-207.756610880363,66.1229203990175,10.3258506102191));
#18743=CARTESIAN_POINT('Ctrl Pts',(-207.436959498352,63.2908826337379,10.4847589290234));
#18744=CARTESIAN_POINT('Ctrl Pts',(-204.883130885644,62.0257445673959,10.6436672478277));
#18745=CARTESIAN_POINT('Ctrl Pts',(-202.436446570756,63.4873706390274,10.802575566632));
#18746=CARTESIAN_POINT('Ctrl Pts',(-202.339999387492,66.3357584024529,10.9614838854363));
#18747=CARTESIAN_POINT('Ctrl Pts',(-204.682211035499,67.9595377920051,11.1203922042407));
#18748=CARTESIAN_POINT('Ctrl Pts',(-207.315768054299,66.870046011989,11.279300523045));
#18749=CARTESIAN_POINT('Ctrl Pts',(-207.826254803778,64.0661169492992,11.4382088418493));
#18750=CARTESIAN_POINT('Ctrl Pts',(-205.74566273762,62.1183614296738,11.5971171606536));
#18751=CARTESIAN_POINT('Ctrl Pts',(-202.98145540773,62.8124599438455,11.7560254794579));
#18752=CARTESIAN_POINT('Ctrl Pts',(-202.067827199178,65.5120707318156,11.9149337982622));
#18753=CARTESIAN_POINT('Ctrl Pts',(-203.84238224213,67.7422207961682,12.0738421170665));
#18754=CARTESIAN_POINT('Ctrl Pts',(-206.678228307043,67.4583334838238,12.2327504358708));
#18755=CARTESIAN_POINT('Ctrl Pts',(-207.975493417271,64.9206735098047,12.3916587546751));
#18756=CARTESIAN_POINT('Ctrl Pts',(-206.544859419016,62.4557391753607,12.5505670734794));
#18757=CARTESIAN_POINT('Ctrl Pts',(-203.697915571989,62.3233547283102,12.7094753922837));
#18758=CARTESIAN_POINT('Ctrl Pts',(-202.044708175418,64.644888749949,12.868383711088));
#18759=CARTESIAN_POINT('Ctrl Pts',(-203.100879292971,67.2919847968046,13.0272920298923));
#18760=CARTESIAN_POINT('Ctrl Pts',(-205.89814304858,67.8378147986296,13.1862003486966));
#18761=CARTESIAN_POINT('Ctrl Pts',(-207.871999295751,65.7819679114821,13.3451086675009));
#18762=CARTESIAN_POINT('Ctrl Pts',(-207.21283868803,63.0092215814544,13.5040169863053));
#18763=CARTESIAN_POINT('Ctrl Pts',(-204.524972304159,62.0615986581739,13.6629253051096));
#18764=CARTESIAN_POINT('Ctrl Pts',(-202.272606001323,63.8078692367045,13.8218336239139));
#18765=CARTESIAN_POINT('Ctrl Pts',(-202.520684035478,66.6470719881461,13.9807419427182));
#18766=CARTESIAN_POINT('Ctrl Pts',(-205.041771229913,67.9762575224163,14.1396502615225));
#18767=CARTESIAN_POINT('Ctrl Pts',(-207.524563038319,66.5768434816013,14.2985585803268));
#18768=CARTESIAN_POINT('Ctrl Pts',(-207.692863647714,63.7317968446979,14.4574668991311));
#18769=CARTESIAN_POINT('Ctrl Pts',(-205.392377007752,62.0494249253602,14.6163752179354));
#18770=CARTESIAN_POINT('Ctrl Pts',(-202.732163419374,63.0721067640084,14.7752835367397));
#18771=CARTESIAN_POINT('Ctrl Pts',(-202.151077252885,65.8622605875592,14.934191855544));
#18772=CARTESIAN_POINT('Ctrl Pts',(-204.181851224064,67.8619014547198,15.0931001743483));
#18773=CARTESIAN_POINT('Ctrl Pts',(-206.962695662023,67.2377873514137,15.2520084931526));
#18774=CARTESIAN_POINT('Ctrl Pts',(-207.944160979464,64.562085971191,15.4109168119569));
#18775=CARTESIAN_POINT('Ctrl Pts',(-206.226455863752,62.2878774852072,15.5698251307612));
#18776=CARTESIAN_POINT('Ctrl Pts',(-203.384342624961,62.5000751268878,15.7287334495655));
#18777=CARTESIAN_POINT('Ctrl Pts',(-202.02346061555,65.0042531094591,15.8876417683698));
#18778=CARTESIAN_POINT('Ctrl Pts',(-203.391406578293,67.504373050753,16.0465500871742));
#18779=CARTESIAN_POINT('Ctrl Pts',(-206.234154908835,67.7088387528733,16.2054584059785));
#18780=CARTESIAN_POINT('Ctrl Pts',(-207.945316421862,65.4291981922897,16.3643667247828));
#18781=CARTESIAN_POINT('Ctrl Pts',(-206.956507284456,62.7574592385606,16.5232750435871));
#18782=CARTESIAN_POINT('Ctrl Pts',(-204.173461846155,62.1387919626312,16.6821833623914));
#18783=CARTESIAN_POINT('Ctrl Pts',(-202.149338134461,64.1491415855772,16.8410916811957));
#18784=CARTESIAN_POINT('Ctrl Pts',(-202.542049969887,65.9991535645903,16.9470305603986));
#18785=CARTESIAN_POINT('Ctrl Pts',(-203.086534003335,66.6359872033749,17.));
#18786=CARTESIAN_POINT('Ctrl Pts',(-202.485823128102,65.0013539996937,0.887416697508052));
#18787=CARTESIAN_POINT('Ctrl Pts',(-202.484195200284,65.3337573103262,0.908364398593722));
#18788=CARTESIAN_POINT('Ctrl Pts',(-202.545417687543,65.6655864079193,0.929312099679392));
#18789=CARTESIAN_POINT('Ctrl Pts',(-202.672298789244,65.9700517898377,0.950259800765062));
#18790=CARTESIAN_POINT('Ctrl Pts',(-202.993136900579,66.7399386901854,1.0032292403665));
#18791=CARTESIAN_POINT('Ctrl Pts',(-203.733801401561,67.3348598216632,1.05619867996793));
#18792=CARTESIAN_POINT('Ctrl Pts',(-204.554762020693,67.4821203593099,1.10916811956937));
#18793=CARTESIAN_POINT('Ctrl Pts',(-205.375722639825,67.6293808969566,1.1621375591708));
#18794=CARTESIAN_POINT('Ctrl Pts',(-206.276979377107,67.3289808407722,1.21510699877224));
#18795=CARTESIAN_POINT('Ctrl Pts',(-206.845407885986,66.7186152441669,1.26807643837368));
#18796=CARTESIAN_POINT('Ctrl Pts',(-207.413836394865,66.1082496475615,1.32104587797511));
#18797=CARTESIAN_POINT('Ctrl Pts',(-207.649436675341,65.187918510535,1.37401531757655));
#18798=CARTESIAN_POINT('Ctrl Pts',(-207.444207618282,64.3794997152261,1.42698475717798));
#18799=CARTESIAN_POINT('Ctrl Pts',(-207.238978561223,63.5710809199172,1.47995419677942));
#18800=CARTESIAN_POINT('Ctrl Pts',(-206.592920166629,62.8745744663259,1.53292363638085));
#18801=CARTESIAN_POINT('Ctrl Pts',(-205.80218357439,62.6092534503727,1.58589307598229));
#18802=CARTESIAN_POINT('Ctrl Pts',(-205.011446982151,62.3439324344196,1.63886251558373));
#18803=CARTESIAN_POINT('Ctrl Pts',(-204.076032192267,62.5097968561048,1.69183195518516));
#18804=CARTESIAN_POINT('Ctrl Pts',(-203.424727348351,63.0308161541245,1.7448013947866));
#18805=CARTESIAN_POINT('Ctrl Pts',(-202.840201389118,63.4984148643111,1.79233982902708));
#18806=CARTESIAN_POINT('Ctrl Pts',(-202.48451199895,64.2520733360095,1.83987826326757));
#18807=CARTESIAN_POINT('Ctrl Pts',(-202.479332509853,65.0014637523716,1.88741669750805));
#18808=CARTESIAN_POINT('Ctrl Pts',(-204.206200717467,62.0307770462543,-5.55111512312578E-16));
#18809=CARTESIAN_POINT('Ctrl Pts',(-204.113162249417,62.0648109334671,-5.19915500288305E-16));
#18810=CARTESIAN_POINT('Ctrl Pts',(-204.02219118159,62.1036166453176,-4.84452877073069E-16));
#18811=CARTESIAN_POINT('Ctrl Pts',(-203.93349495337,62.1468647837849,-4.82253126321552E-16));
#18812=CARTESIAN_POINT('Ctrl Pts',(-203.842820762435,62.1910773736963,-4.80004320214958E-16));
#18813=CARTESIAN_POINT('Ctrl Pts',(-203.754523335469,62.239933353,-9.13199113811134E-16));
#18814=CARTESIAN_POINT('Ctrl Pts',(-203.668853233392,62.2931263628092,-1.02001740387436E-15));
#18815=CARTESIAN_POINT('Ctrl Pts',(-203.585825130324,62.3446789417594,-1.1235415013366E-15));
#18816=CARTESIAN_POINT('Ctrl Pts',(-203.505264469594,62.4003060362145,-6.67670990993899E-16));
#18817=CARTESIAN_POINT('Ctrl Pts',(-203.42743316137,62.4597595642908,-7.49400541621981E-16));
#18818=CARTESIAN_POINT('Ctrl Pts',(-203.359330766673,62.5117814013576,-8.20913898421552E-16));
#18819=CARTESIAN_POINT('Ctrl Pts',(-203.293318330331,62.5667335723465,-9.45964652035114E-16));
#18820=CARTESIAN_POINT('Ctrl Pts',(-203.229596673155,62.6244628960252,-9.78384040450919E-16));
#18821=CARTESIAN_POINT('Ctrl Pts',(-203.216348740433,62.6364650037874,-9.85124133155235E-16));
#18822=CARTESIAN_POINT('Ctrl Pts',(-203.203198172353,62.6485889403755,-3.4496231498821E-16));
#18823=CARTESIAN_POINT('Ctrl Pts',(-203.190163654011,62.6608172960224,-3.46944695195361E-16));
#18824=CARTESIAN_POINT('Ctrl Pts',(-203.11774011012,62.7287615674313,-3.57959371470727E-16));
#18825=CARTESIAN_POINT('Ctrl Pts',(-203.048782373238,62.8000276808216,-5.09072278378989E-16));
#18826=CARTESIAN_POINT('Ctrl Pts',(-202.983529572481,62.8743236281409,-5.13478148889135E-16));
#18827=CARTESIAN_POINT('Ctrl Pts',(-202.918635349275,62.9482113039592,-5.17859808235267E-16));
#18828=CARTESIAN_POINT('Ctrl Pts',(-202.857404970179,63.0250964056677,-2.66956613222884E-16));
#18829=CARTESIAN_POINT('Ctrl Pts',(-202.800117264857,63.1047184530433,-2.22044604925031E-16));
#18830=CARTESIAN_POINT('Ctrl Pts',(-202.744165764651,63.1824833587091,-1.78180145222485E-16));
#18831=CARTESIAN_POINT('Ctrl Pts',(-202.691974876248,63.2628597651003,-1.00656795420818E-15));
#18832=CARTESIAN_POINT('Ctrl Pts',(-202.643851527184,63.3456191713536,-1.0547118733939E-15));
#18833=CARTESIAN_POINT('Ctrl Pts',(-202.623072180899,63.3813541398117,-1.0755001017227E-15));
#18834=CARTESIAN_POINT('Ctrl Pts',(-202.60305183952,63.4175335255461,-2.58501556813931E-16));
#18835=CARTESIAN_POINT('Ctrl Pts',(-202.58381822777,63.454139265439,-1.94289029309402E-16));
#18836=CARTESIAN_POINT('Ctrl Pts',(-202.569903820985,63.480621403177,-1.47834975850494E-16));
#18837=CARTESIAN_POINT('Ctrl Pts',(-202.556401202133,63.5073266847522,-7.93899856949203E-16));
#18838=CARTESIAN_POINT('Ctrl Pts',(-202.5433215057,63.5342482737999,-8.32667268468867E-16));
#18839=CARTESIAN_POINT('Ctrl Pts',(-202.537160097315,63.5469301357491,-8.50929301967292E-16));
#18840=CARTESIAN_POINT('Ctrl Pts',(-202.531094723709,63.5596556012092,-3.63050352889582E-16));
#18841=CARTESIAN_POINT('Ctrl Pts',(-202.525129549917,63.5724168279603,-3.7470027081099E-16));
#18842=CARTESIAN_POINT('Ctrl Pts',(-202.485113190241,63.6580233597082,-4.52851775196109E-16));
#18843=CARTESIAN_POINT('Ctrl Pts',(-202.449555061626,63.7453341587585,2.75905776866127E-16));
#18844=CARTESIAN_POINT('Ctrl Pts',(-202.418706882959,63.8341116308705,2.22044604925031E-16));
#18845=CARTESIAN_POINT('Ctrl Pts',(-202.388542894157,63.9209200840876,1.6937803407733E-16));
#18846=CARTESIAN_POINT('Ctrl Pts',(-202.362882030333,64.0091315459226,-9.1941220868861E-16));
#18847=CARTESIAN_POINT('Ctrl Pts',(-202.342008814717,64.0985324360296,-8.32667268468867E-16));
#18848=CARTESIAN_POINT('Ctrl Pts',(-202.338628814105,64.1130091256228,-8.18620656943663E-16));
#18849=CARTESIAN_POINT('Ctrl Pts',(-202.335374462847,64.1275170099365,-5.95910370058754E-16));
#18850=CARTESIAN_POINT('Ctrl Pts',(-202.332247099787,64.1420551858173,-5.82867087928207E-16));
#18851=CARTESIAN_POINT('Ctrl Pts',(-202.312208792581,64.2352072851979,-4.99293390427251E-16));
#18852=CARTESIAN_POINT('Ctrl Pts',(-202.297379875413,64.3296040558921,-8.33690503982433E-17));
#18853=CARTESIAN_POINT('Ctrl Pts',(-202.287681750639,64.4248371114872,-5.55111512312578E-17));
#18854=CARTESIAN_POINT('Ctrl Pts',(-202.284325955759,64.4577901418682,-4.58716180684954E-17));
#18855=CARTESIAN_POINT('Ctrl Pts',(-202.28158492797,64.4908431751708,-8.28167483116791E-16));
#18856=CARTESIAN_POINT('Ctrl Pts',(-202.279456765112,64.5239787674251,-8.60422844084496E-16));
#18857=CARTESIAN_POINT('Ctrl Pts',(-202.278429684535,64.5399704586003,-8.75989723570996E-16));
#18858=CARTESIAN_POINT('Ctrl Pts',(-202.277545359971,64.555981373961,-8.02943466711267E-16));
#18859=CARTESIAN_POINT('Ctrl Pts',(-202.276803632431,64.5720095213841,-8.04911692853238E-16));
#18860=CARTESIAN_POINT('Ctrl Pts',(-202.276227016754,64.5844697315966,-8.06441783064374E-16));
#18861=CARTESIAN_POINT('Ctrl Pts',(-202.275736678019,64.5969392095638,-5.87596457671717E-16));
#18862=CARTESIAN_POINT('Ctrl Pts',(-202.275332691875,64.6094071262613,-5.82867087928207E-16));
#18863=CARTESIAN_POINT('Ctrl Pts',(-202.272313622363,64.702582369262,-5.47523558950325E-16));
#18864=CARTESIAN_POINT('Ctrl Pts',(-202.27410534735,64.7958212167759,-9.81423475480654E-16));
#18865=CARTESIAN_POINT('Ctrl Pts',(-202.280568163262,64.8887492259718,-9.15933995315754E-16));
#18866=CARTESIAN_POINT('Ctrl Pts',(-202.28704447601,64.9818713044648,-8.50307748018024E-16));
#18867=CARTESIAN_POINT('Ctrl Pts',(-202.298211793817,65.0746822257257,-8.07734983664408E-16));
#18868=CARTESIAN_POINT('Ctrl Pts',(-202.313980610279,65.1667932227156,-7.49400541621981E-16));
#18869=CARTESIAN_POINT('Ctrl Pts',(-202.329528117816,65.257611479329,-6.91884799745999E-16));
#18870=CARTESIAN_POINT('Ctrl Pts',(-202.349549338359,65.3477501671012,-2.84670909400231E-16));
#18871=CARTESIAN_POINT('Ctrl Pts',(-202.374001557502,65.4368115389553,-1.94289029309402E-16));
#18872=CARTESIAN_POINT('Ctrl Pts',(-202.383514216169,65.4714591276246,-1.59127722680513E-16));
#18873=CARTESIAN_POINT('Ctrl Pts',(-202.393697911918,65.5059433314471,-4.85030275451525E-16));
#18874=CARTESIAN_POINT('Ctrl Pts',(-202.404551700249,65.5402392680712,-4.71844785465692E-16));
#18875=CARTESIAN_POINT('Ctrl Pts',(-202.410350726718,65.5585631047066,-4.64799963593452E-16));
#18876=CARTESIAN_POINT('Ctrl Pts',(-202.41634105309,65.5768331827315,-6.36029965202052E-16));
#18877=CARTESIAN_POINT('Ctrl Pts',(-202.422522630952,65.5950455929995,-6.38378239159465E-16));
#18878=CARTESIAN_POINT('Ctrl Pts',(-202.428041241916,65.6113047438546,-6.40474663518505E-16));
#18879=CARTESIAN_POINT('Ctrl Pts',(-202.433712823702,65.6275191792443,-1.66152285628493E-16));
#18880=CARTESIAN_POINT('Ctrl Pts',(-202.43953101583,65.6436691493443,-1.66533453693773E-16));
#18881=CARTESIAN_POINT('Ctrl Pts',(-202.470364649952,65.7292562627001,-1.68553462041071E-16));
#18882=CARTESIAN_POINT('Ctrl Pts',(-202.505348644146,65.8131450789626,4.41371823884456E-16));
#18883=CARTESIAN_POINT('Ctrl Pts',(-202.544418722017,65.8949548979899,0.));
#18884=CARTESIAN_POINT('Ctrl Pts',(-202.575881626623,65.9608358655278,-3.55434141613069E-16));
#18885=CARTESIAN_POINT('Ctrl Pts',(-202.609995265414,66.0253683017606,-7.18594950445821E-16));
#18886=CARTESIAN_POINT('Ctrl Pts',(-202.646744272941,66.0883356853988,-5.55111512312578E-16));
#18887=CARTESIAN_POINT('Ctrl Pts',(-202.661986555904,66.1144524908179,-4.87303944389755E-16));
#18888=CARTESIAN_POINT('Ctrl Pts',(-202.677682386268,66.1402998412242,-7.97734533373392E-16));
#18889=CARTESIAN_POINT('Ctrl Pts',(-202.69383140079,66.1658612939494,-7.7715611723761E-16));
#18890=CARTESIAN_POINT('Ctrl Pts',(-202.702298041279,66.1792627080302,-7.66367220427743E-16));
#18891=CARTESIAN_POINT('Ctrl Pts',(-202.710887832138,66.1925831745098,-5.40710766792841E-17));
#18892=CARTESIAN_POINT('Ctrl Pts',(-202.719595914358,66.2058134485369,-1.11022302462516E-16));
#18893=CARTESIAN_POINT('Ctrl Pts',(-202.767005259998,66.2778429285551,-4.21081426798669E-16));
#18894=CARTESIAN_POINT('Ctrl Pts',(-202.817957067113,66.3472640345857,-9.3988901168733E-16));
#18895=CARTESIAN_POINT('Ctrl Pts',(-202.87241461149,66.4137214114329,-7.7715611723761E-16));
#18896=CARTESIAN_POINT('Ctrl Pts',(-202.926872155867,66.4801787882801,-6.14423222787889E-16));
#18897=CARTESIAN_POINT('Ctrl Pts',(-202.984835768426,66.5436731279146,-3.7164630165585E-17));
#18898=CARTESIAN_POINT('Ctrl Pts',(-203.04629821927,66.6038050748561,-2.22044604925031E-16));
#18899=CARTESIAN_POINT('Ctrl Pts',(-203.058349034853,66.6155950212913,-2.58104842041481E-16));
#18900=CARTESIAN_POINT('Ctrl Pts',(-203.070534438641,66.627255553132,-2.14870316912335E-16));
#18901=CARTESIAN_POINT('Ctrl Pts',(-203.082851846776,66.6387856087136,-2.22044604925031E-16));
#18902=CARTESIAN_POINT('Origin',(-205.,65.,9.));
#18903=CARTESIAN_POINT('Origin',(-205.,-95.,17.));
#18904=CARTESIAN_POINT('Ctrl Pts',(-203.086534003335,-93.3640127966251,
17.));
#18905=CARTESIAN_POINT('Ctrl Pts',(-203.024408000274,-93.4223959843149,
17.));
#18906=CARTESIAN_POINT('Ctrl Pts',(-202.965660700181,-93.4840340445169,
17.));
#18907=CARTESIAN_POINT('Ctrl Pts',(-202.910302663152,-93.5485502404793,
17.));
#18908=CARTESIAN_POINT('Ctrl Pts',(-202.85358729986,-93.6146483120265,17.));
#18909=CARTESIAN_POINT('Ctrl Pts',(-202.800428974214,-93.6837678789023,
17.));
#18910=CARTESIAN_POINT('Ctrl Pts',(-202.750867981151,-93.7555500875478,
17.));
#18911=CARTESIAN_POINT('Ctrl Pts',(-202.737959277062,-93.7742465508953,
17.));
#18912=CARTESIAN_POINT('Ctrl Pts',(-202.725294786098,-93.7931238635411,
17.));
#18913=CARTESIAN_POINT('Ctrl Pts',(-202.712875593634,-93.8121761152587,
17.));
#18914=CARTESIAN_POINT('Ctrl Pts',(-202.702666953263,-93.8278371646063,
17.));
#18915=CARTESIAN_POINT('Ctrl Pts',(-202.692623587495,-93.8436173779436,
17.));
#18916=CARTESIAN_POINT('Ctrl Pts',(-202.682755039166,-93.8594987232582,
17.));
#18917=CARTESIAN_POINT('Ctrl Pts',(-202.635325956578,-93.9358258195438,
17.));
#18918=CARTESIAN_POINT('Ctrl Pts',(-202.591881662897,-94.014561411206,17.));
#18919=CARTESIAN_POINT('Ctrl Pts',(-202.552455307866,-94.0953124442998,
17.));
#18920=CARTESIAN_POINT('Ctrl Pts',(-202.520329580588,-94.1611107070231,
17.));
#18921=CARTESIAN_POINT('Ctrl Pts',(-202.49087203172,-94.2282482025802,17.));
#18922=CARTESIAN_POINT('Ctrl Pts',(-202.464118359925,-94.2965306954245,
17.));
#18923=CARTESIAN_POINT('Ctrl Pts',(-202.455239584334,-94.3191916944583,
17.));
#18924=CARTESIAN_POINT('Ctrl Pts',(-202.446658750236,-94.3419789158481,
17.));
#18925=CARTESIAN_POINT('Ctrl Pts',(-202.4383775944,-94.3648855717116,17.));
#18926=CARTESIAN_POINT('Ctrl Pts',(-202.431690779773,-94.3833820913431,
17.));
#18927=CARTESIAN_POINT('Ctrl Pts',(-202.425198561125,-94.4019592233538,
17.));
#18928=CARTESIAN_POINT('Ctrl Pts',(-202.418909543929,-94.4205899139815,
17.));
#18929=CARTESIAN_POINT('Ctrl Pts',(-202.389394386736,-94.5080261135151,
17.));
#18930=CARTESIAN_POINT('Ctrl Pts',(-202.364312756292,-94.5967429324199,
17.));
#18931=CARTESIAN_POINT('Ctrl Pts',(-202.343695730977,-94.6863420431789,
17.));
#18932=CARTESIAN_POINT('Ctrl Pts',(-202.322620129767,-94.7779340695863,
17.));
#18933=CARTESIAN_POINT('Ctrl Pts',(-202.306209395933,-94.8704488625012,
17.));
#18934=CARTESIAN_POINT('Ctrl Pts',(-202.294539564163,-94.9634948472204,
17.));
#18935=CARTESIAN_POINT('Ctrl Pts',(-202.283037042173,-95.0552068364273,
17.));
#18936=CARTESIAN_POINT('Ctrl Pts',(-202.27614016437,-95.1474358567499,17.));
#18937=CARTESIAN_POINT('Ctrl Pts',(-202.273968836359,-95.2398261209644,
17.));
#18938=CARTESIAN_POINT('Ctrl Pts',(-202.272844366773,-95.2876724351408,
17.));
#18939=CARTESIAN_POINT('Ctrl Pts',(-202.272988049685,-95.3355622217538,
17.));
#18940=CARTESIAN_POINT('Ctrl Pts',(-202.274422018419,-95.3834468414973,
17.));
#18941=CARTESIAN_POINT('Ctrl Pts',(-202.275072129396,-95.4051560435378,
17.));
#18942=CARTESIAN_POINT('Ctrl Pts',(-202.275988023267,-95.4268712623304,
17.));
#18943=CARTESIAN_POINT('Ctrl Pts',(-202.277169537603,-95.4485498237118,
17.));
#18944=CARTESIAN_POINT('Ctrl Pts',(-202.282380920127,-95.544168871676,17.));
#18945=CARTESIAN_POINT('Ctrl Pts',(-202.29275597009,-95.63918004578,17.));
#18946=CARTESIAN_POINT('Ctrl Pts',(-202.308361643616,-95.7331861624806,
17.));
#18947=CARTESIAN_POINT('Ctrl Pts',(-202.312210372873,-95.7563703006822,
17.));
#18948=CARTESIAN_POINT('Ctrl Pts',(-202.316377475622,-95.7794934013305,
17.));
#18949=CARTESIAN_POINT('Ctrl Pts',(-202.320864419024,-95.8025496616774,
17.));
#18950=CARTESIAN_POINT('Ctrl Pts',(-202.338369892673,-95.8925019347234,
17.));
#18951=CARTESIAN_POINT('Ctrl Pts',(-202.360739472015,-95.9814367403613,
17.));
#18952=CARTESIAN_POINT('Ctrl Pts',(-202.387670003523,-96.0691240547554,
17.));
#18953=CARTESIAN_POINT('Ctrl Pts',(-202.415202635706,-96.1587718425676,
17.));
#18954=CARTESIAN_POINT('Ctrl Pts',(-202.447502661721,-96.2471164356113,
17.));
#18955=CARTESIAN_POINT('Ctrl Pts',(-202.484300312417,-96.3339075926369,
17.));
#18956=CARTESIAN_POINT('Ctrl Pts',(-202.498927651313,-96.3684077208491,
17.));
#18957=CARTESIAN_POINT('Ctrl Pts',(-202.514266241852,-96.4026622798363,
17.));
#18958=CARTESIAN_POINT('Ctrl Pts',(-202.530301312039,-96.4366549706656,
17.));
#18959=CARTESIAN_POINT('Ctrl Pts',(-202.538298082829,-96.453607297903,17.));
#18960=CARTESIAN_POINT('Ctrl Pts',(-202.546469923465,-96.4704979563681,
17.));
#18961=CARTESIAN_POINT('Ctrl Pts',(-202.554802687444,-96.4873005192782,
17.));
#18962=CARTESIAN_POINT('Ctrl Pts',(-202.597597092774,-96.5735930975321,
17.));
#18963=CARTESIAN_POINT('Ctrl Pts',(-202.644686646802,-96.6576840525218,
17.));
#18964=CARTESIAN_POINT('Ctrl Pts',(-202.695725951514,-96.7393268492994,
17.));
#18965=CARTESIAN_POINT('Ctrl Pts',(-202.747782191651,-96.8225963424571,
17.));
#18966=CARTESIAN_POINT('Ctrl Pts',(-202.803947462512,-96.9033199151229,
17.));
#18967=CARTESIAN_POINT('Ctrl Pts',(-202.863910401783,-96.9812287996324,
17.));
#18968=CARTESIAN_POINT('Ctrl Pts',(-202.924370848883,-97.0597840880771,
17.));
#18969=CARTESIAN_POINT('Ctrl Pts',(-202.988692707376,-97.1354786200808,
17.));
#18970=CARTESIAN_POINT('Ctrl Pts',(-203.056606164229,-97.2080175007534,
17.));
#18971=CARTESIAN_POINT('Ctrl Pts',(-203.094651211644,-97.2486537057484,
17.));
#18972=CARTESIAN_POINT('Ctrl Pts',(-203.133824229424,-97.288299178605,17.));
#18973=CARTESIAN_POINT('Ctrl Pts',(-203.174083617339,-97.3268979340229,
17.));
#18974=CARTESIAN_POINT('Ctrl Pts',(-203.185629855,-97.3379679086686,17.));
#18975=CARTESIAN_POINT('Ctrl Pts',(-203.197265472916,-97.3489517664843,
17.));
#18976=CARTESIAN_POINT('Ctrl Pts',(-203.208989546289,-97.3598481307381,
17.));
#18977=CARTESIAN_POINT('Ctrl Pts',(-203.219402554585,-97.3695259899387,
17.));
#18978=CARTESIAN_POINT('Ctrl Pts',(-203.22988211016,-97.3791317753717,17.));
#18979=CARTESIAN_POINT('Ctrl Pts',(-203.240421391601,-97.3886593080805,
17.));
#18980=CARTESIAN_POINT('Ctrl Pts',(-203.316131451988,-97.4571013627712,
17.));
#18981=CARTESIAN_POINT('Ctrl Pts',(-203.395010716132,-97.5215917702376,
17.));
#18982=CARTESIAN_POINT('Ctrl Pts',(-203.47672873235,-97.5818514569894,17.));
#18983=CARTESIAN_POINT('Ctrl Pts',(-203.558539296836,-97.6421793897639,
17.));
#18984=CARTESIAN_POINT('Ctrl Pts',(-203.64319562843,-97.6982678463519,17.));
#18985=CARTESIAN_POINT('Ctrl Pts',(-203.730411362481,-97.7498108582678,
17.));
#18986=CARTESIAN_POINT('Ctrl Pts',(-203.815808401538,-97.8002790524476,
17.));
#18987=CARTESIAN_POINT('Ctrl Pts',(-203.903659887931,-97.8463900605495,
17.));
#18988=CARTESIAN_POINT('Ctrl Pts',(-203.993730815686,-97.8878209215619,
17.));
#18989=CARTESIAN_POINT('Ctrl Pts',(-204.044096679879,-97.9109882317155,
17.));
#18990=CARTESIAN_POINT('Ctrl Pts',(-204.095157077275,-97.9326914441169,
17.));
#18991=CARTESIAN_POINT('Ctrl Pts',(-204.146874513566,-97.9528678786509,
17.));
#18992=CARTESIAN_POINT('Ctrl Pts',(-204.165970747425,-97.9603178595455,
17.));
#18993=CARTESIAN_POINT('Ctrl Pts',(-204.185156583856,-97.9675596309774,
17.));
#18994=CARTESIAN_POINT('Ctrl Pts',(-204.204429055805,-97.9745938792693,
17.));
#18995=CARTESIAN_POINT('Ctrl Pts',(-205.793799282533,-97.9692229537457,
17.));
#18996=CARTESIAN_POINT('Ctrl Pts',(-205.888625424821,-97.9345351273112,
17.));
#18997=CARTESIAN_POINT('Ctrl Pts',(-205.981405808652,-97.8948521769808,
17.));
#18998=CARTESIAN_POINT('Ctrl Pts',(-206.07190060029,-97.8504957325714,17.));
#18999=CARTESIAN_POINT('Ctrl Pts',(-206.163681990447,-97.8055086558944,
17.));
#19000=CARTESIAN_POINT('Ctrl Pts',(-206.253113003673,-97.7557135474638,
17.));
#19001=CARTESIAN_POINT('Ctrl Pts',(-206.339909395556,-97.7014052421032,
17.));
#19002=CARTESIAN_POINT('Ctrl Pts',(-206.36428919546,-97.6861508566487,17.));
#19003=CARTESIAN_POINT('Ctrl Pts',(-206.388460895741,-97.6705401887824,
17.));
#19004=CARTESIAN_POINT('Ctrl Pts',(-206.412417611516,-97.6545793244046,
17.));
#19005=CARTESIAN_POINT('Ctrl Pts',(-206.431857056321,-97.6416280357124,
17.));
#19006=CARTESIAN_POINT('Ctrl Pts',(-206.451157156149,-97.6284444656715,
17.));
#19007=CARTESIAN_POINT('Ctrl Pts',(-206.470294679557,-97.615045820576,17.));
#19008=CARTESIAN_POINT('Ctrl Pts',(-206.55300602175,-97.5571376003872,17.));
#19009=CARTESIAN_POINT('Ctrl Pts',(-206.632761459732,-97.4951644765478,
17.));
#19010=CARTESIAN_POINT('Ctrl Pts',(-206.709295581515,-97.4294253116699,
17.));
#19011=CARTESIAN_POINT('Ctrl Pts',(-206.76882353903,-97.3782936318028,17.));
#19012=CARTESIAN_POINT('Ctrl Pts',(-206.82640208509,-97.324882704478,17.));
#19013=CARTESIAN_POINT('Ctrl Pts',(-206.881888208557,-97.2693210301885,
17.));
#19014=CARTESIAN_POINT('Ctrl Pts',(-206.912065000132,-97.2391031493952,
17.));
#19015=CARTESIAN_POINT('Ctrl Pts',(-206.941622589496,-97.2082489492308,
17.));
#19016=CARTESIAN_POINT('Ctrl Pts',(-206.970535716259,-97.1767781813433,
17.));
#19017=CARTESIAN_POINT('Ctrl Pts',(-206.982341010226,-97.163928596816,17.));
#19018=CARTESIAN_POINT('Ctrl Pts',(-206.994033762366,-97.1509816881149,
17.));
#19019=CARTESIAN_POINT('Ctrl Pts',(-207.0056075954,-97.1379446989878,17.));
#19020=CARTESIAN_POINT('Ctrl Pts',(-207.071007089784,-97.0642774450467,
17.));
#19021=CARTESIAN_POINT('Ctrl Pts',(-207.132664401507,-96.9876805132482,
17.));
#19022=CARTESIAN_POINT('Ctrl Pts',(-207.190334415737,-96.9084322842349,
17.));
#19023=CARTESIAN_POINT('Ctrl Pts',(-207.247546870099,-96.8298128188818,
17.));
#19024=CARTESIAN_POINT('Ctrl Pts',(-207.300835489002,-96.7485831773063,
17.));
#19025=CARTESIAN_POINT('Ctrl Pts',(-207.349914644925,-96.6649933299702,
17.));
#19026=CARTESIAN_POINT('Ctrl Pts',(-207.397475414546,-96.5839895433924,
17.));
#19027=CARTESIAN_POINT('Ctrl Pts',(-207.441083337704,-96.5007686302,17.));
#19028=CARTESIAN_POINT('Ctrl Pts',(-207.480430575245,-96.4155483735031,
17.));
#19029=CARTESIAN_POINT('Ctrl Pts',(-207.501046319853,-96.3708977408989,
17.));
#19030=CARTESIAN_POINT('Ctrl Pts',(-207.520491610764,-96.3256981540745,
17.));
#19031=CARTESIAN_POINT('Ctrl Pts',(-207.538716406462,-96.2799807651805,
17.));
#19032=CARTESIAN_POINT('Ctrl Pts',(-207.545013455281,-96.2641844492984,
17.));
#19033=CARTESIAN_POINT('Ctrl Pts',(-207.551164759148,-96.2483263172452,
17.));
#19034=CARTESIAN_POINT('Ctrl Pts',(-207.557168136471,-96.2324076615222,
17.));
#19035=CARTESIAN_POINT('Ctrl Pts',(-207.562729489382,-96.2176610851248,
17.));
#19036=CARTESIAN_POINT('Ctrl Pts',(-207.568161126813,-96.2028697871422,
17.));
#19037=CARTESIAN_POINT('Ctrl Pts',(-207.573459223174,-96.1880421233524,
17.));
#19038=CARTESIAN_POINT('Ctrl Pts',(-207.604693505319,-96.1006274365002,
17.));
#19039=CARTESIAN_POINT('Ctrl Pts',(-207.631320267415,-96.011871227871,17.));
#19040=CARTESIAN_POINT('Ctrl Pts',(-207.653087285252,-95.9219972305274,
17.));
#19041=CARTESIAN_POINT('Ctrl Pts',(-207.658248202749,-95.9006882809563,
17.));
#19042=CARTESIAN_POINT('Ctrl Pts',(-207.663135701564,-95.8793164527878,
17.));
#19043=CARTESIAN_POINT('Ctrl Pts',(-207.667745988914,-95.8578846668755,
17.));
#19044=CARTESIAN_POINT('Ctrl Pts',(-207.687556304037,-95.7657926994287,
17.));
#19045=CARTESIAN_POINT('Ctrl Pts',(-207.702252299247,-95.6725932801944,
17.));
#19046=CARTESIAN_POINT('Ctrl Pts',(-207.711945419972,-95.5786784812294,
17.));
#19047=CARTESIAN_POINT('Ctrl Pts',(-207.722114123792,-95.4801558483222,
17.));
#19048=CARTESIAN_POINT('Ctrl Pts',(-207.726777009354,-95.3808446338519,
17.));
#19049=CARTESIAN_POINT('Ctrl Pts',(-207.726004467722,-95.2812134714913,
17.));
#19050=CARTESIAN_POINT('Ctrl Pts',(-207.725764520937,-95.2502686315798,
17.));
#19051=CARTESIAN_POINT('Ctrl Pts',(-207.724999819215,-95.2192931170245,
17.));
#19052=CARTESIAN_POINT('Ctrl Pts',(-207.723711405485,-95.1883015738151,
17.));
#19053=CARTESIAN_POINT('Ctrl Pts',(-207.723122799525,-95.1741432280866,
17.));
#19054=CARTESIAN_POINT('Ctrl Pts',(-207.722424806131,-95.1599814556,17.));
#19055=CARTESIAN_POINT('Ctrl Pts',(-207.721618537088,-95.1458321747028,
17.));
#19056=CARTESIAN_POINT('Ctrl Pts',(-207.716327423532,-95.052977993351,17.));
#19057=CARTESIAN_POINT('Ctrl Pts',(-207.706371932179,-94.9605047986718,
17.));
#19058=CARTESIAN_POINT('Ctrl Pts',(-207.69187986909,-94.8687837046641,17.));
#19059=CARTESIAN_POINT('Ctrl Pts',(-207.67741841215,-94.7772563187229,17.));
#19060=CARTESIAN_POINT('Ctrl Pts',(-207.65843910804,-94.686476913951,17.));
#19061=CARTESIAN_POINT('Ctrl Pts',(-207.635020232395,-94.5968312210243,
17.));
#19062=CARTESIAN_POINT('Ctrl Pts',(-207.611996283944,-94.5086972796644,
17.));
#19063=CARTESIAN_POINT('Ctrl Pts',(-207.584680760938,-94.4216583490485,
17.));
#19064=CARTESIAN_POINT('Ctrl Pts',(-207.553107666477,-94.3361100984335,
17.));
#19065=CARTESIAN_POINT('Ctrl Pts',(-207.536805014678,-94.2919375722512,
17.));
#19066=CARTESIAN_POINT('Ctrl Pts',(-207.519366617313,-94.248163031905,17.));
#19067=CARTESIAN_POINT('Ctrl Pts',(-207.500793443899,-94.2048450949011,
17.));
#19068=CARTESIAN_POINT('Ctrl Pts',(-207.494983237603,-94.1912940368956,
17.));
#19069=CARTESIAN_POINT('Ctrl Pts',(-207.489061191608,-94.1777859684221,
17.));
#19070=CARTESIAN_POINT('Ctrl Pts',(-207.483029722208,-94.1643281685061,
17.));
#19071=CARTESIAN_POINT('Ctrl Pts',(-207.446486020386,-94.0827895259774,
17.));
#19072=CARTESIAN_POINT('Ctrl Pts',(-207.406052561607,-94.0033669713649,
17.));
#19073=CARTESIAN_POINT('Ctrl Pts',(-207.361809047075,-93.9264057217905,
17.));
#19074=CARTESIAN_POINT('Ctrl Pts',(-207.318276162464,-93.85068060744,17.));
#19075=CARTESIAN_POINT('Ctrl Pts',(-207.271054166029,-93.7773376777461,
17.));
#19076=CARTESIAN_POINT('Ctrl Pts',(-207.220181837178,-93.7067387347045,
17.));
#19077=CARTESIAN_POINT('Ctrl Pts',(-207.170938074568,-93.6383998622723,
17.));
#19078=CARTESIAN_POINT('Ctrl Pts',(-207.11827349102,-93.5726316597938,17.));
#19079=CARTESIAN_POINT('Ctrl Pts',(-207.062195033272,-93.5098014324231,
17.));
#19080=CARTESIAN_POINT('Ctrl Pts',(-207.027351929298,-93.4707632663797,
17.));
#19081=CARTESIAN_POINT('Ctrl Pts',(-206.991190374561,-93.4328600994283,
17.));
#19082=CARTESIAN_POINT('Ctrl Pts',(-206.953707394001,-93.3961891492629,
17.));
#19083=CARTESIAN_POINT('Ctrl Pts',(-206.941658629391,-93.3844014088023,
17.));
#19084=CARTESIAN_POINT('Ctrl Pts',(-206.929473297568,-93.3727410508926,
17.));
#19085=CARTESIAN_POINT('Ctrl Pts',(-206.91715387718,-93.3612092940949,17.));
#19086=CARTESIAN_POINT('Origin',(-205.,-95.,-2.20842344717744));
#19087=CARTESIAN_POINT('Ctrl Pts',(-201.92372071423,-94.9977231567353,0.291576552822548));
#19088=CARTESIAN_POINT('Ctrl Pts',(-201.922485530331,-94.8497454287996,
0.299259877064297));
#19089=CARTESIAN_POINT('Ctrl Pts',(-201.999542171248,-93.6828631526875,
0.359912640907482));
#19090=CARTESIAN_POINT('Ctrl Pts',(-203.493268957345,-91.692897649157,0.473534844352101));
#19091=CARTESIAN_POINT('Ctrl Pts',(-206.963866039577,-91.9425114466253,
0.632443163156408));
#19092=CARTESIAN_POINT('Ctrl Pts',(-208.633932755097,-94.9948094985304,
0.791351481960715));
#19093=CARTESIAN_POINT('Ctrl Pts',(-206.972489195327,-98.0520533654047,
0.950259800765021));
#19094=CARTESIAN_POINT('Ctrl Pts',(-203.502670888945,-98.3111182651998,
1.10916811956933));
#19095=CARTESIAN_POINT('Ctrl Pts',(-202.001245999945,-96.3232598794757,
1.22294037025517));
#19096=CARTESIAN_POINT('Ctrl Pts',(-201.922516561303,-95.1532539549744,
1.28374318133958));
#19097=CARTESIAN_POINT('Ctrl Pts',(-201.923792845874,-95.0023469955484,
1.29157655282255));
#19098=CARTESIAN_POINT('Ctrl Pts',(-201.929615858992,-95.0031001153078,
0.208423447177458));
#19099=CARTESIAN_POINT('Ctrl Pts',(-201.934957634602,-94.2978296205795,
0.244887843987843));
#19100=CARTESIAN_POINT('Ctrl Pts',(-202.525017678651,-92.5576756090664,
0.334321680399663));
#19101=CARTESIAN_POINT('Ctrl Pts',(-205.417647323366,-91.3907175644162,
0.476724956412918));
#19102=CARTESIAN_POINT('Ctrl Pts',(-208.260129048284,-93.3950151579563,
0.635633275217225));
#19103=CARTESIAN_POINT('Ctrl Pts',(-208.114979996894,-96.8719144846003,
0.794541594021531));
#19104=CARTESIAN_POINT('Ctrl Pts',(-205.113462590801,-98.6320974631547,
0.953449912825839));
#19105=CARTESIAN_POINT('Ctrl Pts',(-202.417551547519,-97.2695714233959,
1.09141053054448));
#19106=CARTESIAN_POINT('Ctrl Pts',(-201.933583924064,-95.6186998810612,
1.17640170866169));
#19107=CARTESIAN_POINT('Ctrl Pts',(-201.930545885435,-94.9983467356882,
1.20842344717746));
#19108=CARTESIAN_POINT('Ctrl Pts',(-206.913465996665,-93.3640127966251,
0.));
#19109=CARTESIAN_POINT('Ctrl Pts',(-207.457950030113,-94.0008464354096,
0.0529694396014356));
#19110=CARTESIAN_POINT('Ctrl Pts',(-207.850593831989,-95.8509324154922,
0.158908318804306));
#19111=CARTESIAN_POINT('Ctrl Pts',(-205.826561617166,-97.8611954663596,
0.317816637608614));
#19112=CARTESIAN_POINT('Ctrl Pts',(-203.043475003269,-97.2425645771078,
0.47672495641292));
#19113=CARTESIAN_POINT('Ctrl Pts',(-202.054677556737,-94.5707911831857,
0.635633275217227));
#19114=CARTESIAN_POINT('Ctrl Pts',(-203.765838490358,-92.2911566070451,
0.794541594021533));
#19115=CARTESIAN_POINT('Ctrl Pts',(-206.608600212993,-92.4956149558742,
0.95344991282584));
#19116=CARTESIAN_POINT('Ctrl Pts',(-207.976549767678,-94.9957484667481,
1.11235823163015));
#19117=CARTESIAN_POINT('Ctrl Pts',(-206.615663429066,-97.4999330884679,
1.27126655043445));
#19118=CARTESIAN_POINT('Ctrl Pts',(-203.773539600754,-97.7121328233741,
1.43017486923876));
#19119=CARTESIAN_POINT('Ctrl Pts',(-202.055828366454,-95.437915374088,1.58908318804307));
#19120=CARTESIAN_POINT('Ctrl Pts',(-203.037297196393,-92.7622046523681,
1.74799150684737));
#19121=CARTESIAN_POINT('Ctrl Pts',(-205.818151752958,-92.1380880866711,
1.90689982565168));
#19122=CARTESIAN_POINT('Ctrl Pts',(-207.848933088516,-94.1377363167912,
2.06580814445599));
#19123=CARTESIAN_POINT('Ctrl Pts',(-207.267844815878,-96.9279002177238,
2.22471646326029));
#19124=CARTESIAN_POINT('Ctrl Pts',(-204.607621567184,-97.9505857971491,
2.3836247820646));
#19125=CARTESIAN_POINT('Ctrl Pts',(-202.307126575009,-96.2682077551517,
2.54253310086891));
#19126=CARTESIAN_POINT('Ctrl Pts',(-202.475427795301,-93.4231507955679,
2.70144141967322));
#19127=CARTESIAN_POINT('Ctrl Pts',(-204.958228618429,-92.0237316699425,
2.86034973847752));
#19128=CARTESIAN_POINT('Ctrl Pts',(-207.479324966578,-93.3529220322061,
3.01925805728183));
#19129=CARTESIAN_POINT('Ctrl Pts',(-207.727403901463,-96.1921350914307,
3.17816637608613));
#19130=CARTESIAN_POINT('Ctrl Pts',(-205.475029420604,-97.9384120109208,
3.33707469489044));
#19131=CARTESIAN_POINT('Ctrl Pts',(-202.787153277457,-96.9907856467029,
3.49598301369475));
#19132=CARTESIAN_POINT('Ctrl Pts',(-202.127990276418,-94.218029249343,3.65489133249906));
#19133=CARTESIAN_POINT('Ctrl Pts',(-204.101853690385,-92.1621748976358,
3.81379965130336));
#19134=CARTESIAN_POINT('Ctrl Pts',(-206.899127602474,-92.7080068813262,
3.97270797010767));
#19135=CARTESIAN_POINT('Ctrl Pts',(-207.955302554838,-95.3551125394054,
4.13161628891197));
#19136=CARTESIAN_POINT('Ctrl Pts',(-206.3020891557,-97.6766549902215,4.29052460771628));
#19137=CARTESIAN_POINT('Ctrl Pts',(-203.455134971813,-97.5442700624972,
4.44943292652059));
#19138=CARTESIAN_POINT('Ctrl Pts',(-202.024495779124,-95.0793267782196,
4.60834124532489));
#19139=CARTESIAN_POINT('Ctrl Pts',(-203.321765599542,-92.5416575903068,
4.7672495641292));
#19140=CARTESIAN_POINT('Ctrl Pts',(-206.15762196102,-92.2577692472075,4.92615788293351));
#19141=CARTESIAN_POINT('Ctrl Pts',(-207.932183447136,-94.4879274089262,
5.08506620173781));
#19142=CARTESIAN_POINT('Ctrl Pts',(-207.018551921327,-97.1875479988099,
5.24397452054212));
#19143=CARTESIAN_POINT('Ctrl Pts',(-204.254334554982,-97.8816490331574,
5.40288283934643));
#19144=CARTESIAN_POINT('Ctrl Pts',(-202.173734934482,-95.9338864415011,
5.56179115815073));
#19145=CARTESIAN_POINT('Ctrl Pts',(-202.684223537468,-93.1299471981326,
5.72069947695505));
#19146=CARTESIAN_POINT('Ctrl Pts',(-205.317790118349,-92.0404514623223,
5.87960779575934));
#19147=CARTESIAN_POINT('Ctrl Pts',(-207.660010270602,-93.6642367475931,
6.03851611456366));
#19148=CARTESIAN_POINT('Ctrl Pts',(-207.563562737152,-96.5126348531206,
6.19742443336797));
#19149=CARTESIAN_POINT('Ctrl Pts',(-205.116869538691,-97.9742662317143,
6.35633275217226));
#19150=CARTESIAN_POINT('Ctrl Pts',(-202.563031653386,-96.709123571831,6.51524107097658));
#19151=CARTESIAN_POINT('Ctrl Pts',(-202.243379110764,-93.8770755238139,
6.67414938978088));
#19152=CARTESIAN_POINT('Ctrl Pts',(-204.450965789212,-92.0745120848694,
6.83305770858519));
#19153=CARTESIAN_POINT('Ctrl Pts',(-207.161900895669,-92.9540032689432,
6.9919660273895));
#19154=CARTESIAN_POINT('Ctrl Pts',(-207.890829424096,-95.7092413883672,
7.1508743461938));
#19155=CARTESIAN_POINT('Ctrl Pts',(-205.969477846714,-97.8142549299807,
7.30978266499811));
#19156=CARTESIAN_POINT('Ctrl Pts',(-203.159319815119,-97.3391910061333,
7.46869098380242));
#19157=CARTESIAN_POINT('Ctrl Pts',(-202.03667680412,-94.7195829125171,7.62759930260672));
#19158=CARTESIAN_POINT('Ctrl Pts',(-203.630775378654,-92.3570580705415,
7.78650762141103));
#19159=CARTESIAN_POINT('Ctrl Pts',(-206.480163782497,-92.4175528498779,
7.94541594021533));
#19160=CARTESIAN_POINT('Ctrl Pts',(-207.972554574031,-94.8456063129684,
8.10432425901964));
#19161=CARTESIAN_POINT('Ctrl Pts',(-206.739740555722,-97.4152061827031,
8.26323257782395));
#19162=CARTESIAN_POINT('Ctrl Pts',(-203.911951840647,-97.7705720183959,
8.42214089662825));
#19163=CARTESIAN_POINT('Ctrl Pts',(-202.081673517178,-95.5859083937338,
8.58104921543256));
#19164=CARTESIAN_POINT('Ctrl Pts',(-202.926884295628,-92.8640905022736,
8.73995753423686));
#19165=CARTESIAN_POINT('Ctrl Pts',(-205.672704381061,-92.1004505657102,
8.89886585304118));
#19166=CARTESIAN_POINT('Ctrl Pts',(-207.801796608615,-93.995085142839,9.05777417184547));
#19167=CARTESIAN_POINT('Ctrl Pts',(-207.362233020492,-96.8110144292876,
9.2166824906498));
#19168=CARTESIAN_POINT('Ctrl Pts',(-204.757000601372,-97.9666259282991,
9.37559080945408));
#19169=CARTESIAN_POINT('Ctrl Pts',(-202.37454731496,-96.4024679336107,9.53449912825841));
#19170=CARTESIAN_POINT('Ctrl Pts',(-202.399079706051,-93.5525430124821,
9.69340744706271));
#19171=CARTESIAN_POINT('Ctrl Pts',(-204.808106752686,-92.0296304795825,
9.85231576586702));
#19172=CARTESIAN_POINT('Ctrl Pts',(-207.393059383707,-93.2299195237957,
10.0112240846713));
#19173=CARTESIAN_POINT('Ctrl Pts',(-207.784081918476,-96.0529985647693,
10.1701324034756));
#19174=CARTESIAN_POINT('Ctrl Pts',(-205.622689267493,-97.9107002907099,
10.3290407222799));
#19175=CARTESIAN_POINT('Ctrl Pts',(-202.890422055742,-97.0999045224228,
10.4879490410842));
#19176=CARTESIAN_POINT('Ctrl Pts',(-202.09219232497,-94.3639397581774,10.6468573598886));
#19177=CARTESIAN_POINT('Ctrl Pts',(-203.9598081707,-92.211107914521,10.8057656786928));
#19178=CARTESIAN_POINT('Ctrl Pts',(-206.781060259523,-92.6151011639616,
10.9646739974972));
#19179=CARTESIAN_POINT('Ctrl Pts',(-207.969456208958,-95.2055430107611,
11.1235823163015));
#19180=CARTESIAN_POINT('Ctrl Pts',(-206.435487895018,-97.6075453226064,
11.2824906351058));
#19181=CARTESIAN_POINT('Ctrl Pts',(-203.585480323077,-97.6189792266813,
11.4413989539101));
#19182=CARTESIAN_POINT('Ctrl Pts',(-202.032288581145,-95.229362247524,11.6003072727144));
#19183=CARTESIAN_POINT('Ctrl Pts',(-203.199861498522,-92.6294685233712,
11.7592155915187));
#19184=CARTESIAN_POINT('Ctrl Pts',(-206.017781274278,-92.2028515620513,
11.918123910323));
#19185=CARTESIAN_POINT('Ctrl Pts',(-207.902610553307,-94.3406290254934,
12.0770322291273));
#19186=CARTESIAN_POINT('Ctrl Pts',(-207.126358918942,-97.0829104287093,
12.2359405479316));
#19187=CARTESIAN_POINT('Ctrl Pts',(-204.400685193564,-97.9156028311452,
12.3948488667359));
#19188=CARTESIAN_POINT('Ctrl Pts',(-202.224456584312,-96.0753031450743,
12.5537571855402));
#19189=CARTESIAN_POINT('Ctrl Pts',(-202.592815156882,-93.2491775540462,
12.7126655043445));
#19190=CARTESIAN_POINT('Ctrl Pts',(-205.168053889028,-92.0281864128756,
12.8715738231488));
#19191=CARTESIAN_POINT('Ctrl Pts',(-207.58922269399,-93.5317207530604,13.0304821419532));
#19192=CARTESIAN_POINT('Ctrl Pts',(-207.636621072365,-96.3813570961325,
13.1893904607574));
#19193=CARTESIAN_POINT('Ctrl Pts',(-205.266794720449,-97.9645806927232,
13.3482987795618));
#19194=CARTESIAN_POINT('Ctrl Pts',(-202.652373950972,-96.829909844503,13.5072070983661));
#19195=CARTESIAN_POINT('Ctrl Pts',(-202.190230503823,-94.0175981038372,
13.6661154171704));
#19196=CARTESIAN_POINT('Ctrl Pts',(-204.30405232757,-92.1059414404975,13.8250237359747));
#19197=CARTESIAN_POINT('Ctrl Pts',(-207.055911196842,-92.8475253202271,
13.983932054779));
#19198=CARTESIAN_POINT('Ctrl Pts',(-207.922933663676,-95.5624739244494,
14.1428403735833));
#19199=CARTESIAN_POINT('Ctrl Pts',(-206.110243207721,-97.761752729989,14.3017486923876));
#19200=CARTESIAN_POINT('Ctrl Pts',(-203.279694206403,-97.4290874824383,
14.4606570111919));
#19201=CARTESIAN_POINT('Ctrl Pts',(-202.026302290869,-94.869462017148,14.6195653299962));
#19202=CARTESIAN_POINT('Ctrl Pts',(-203.499163277813,-92.4295122395567,
14.7784736488005));
#19203=CARTESIAN_POINT('Ctrl Pts',(-206.347974433471,-92.3461570680267,
14.9373819676048));
#19204=CARTESIAN_POINT('Ctrl Pts',(-207.960978032891,-94.6958151102762,
15.0962902864091));
#19205=CARTESIAN_POINT('Ctrl Pts',(-206.859389366482,-97.3243471311393,
15.2551986052135));
#19206=CARTESIAN_POINT('Ctrl Pts',(-204.053134757144,-97.8219422925345,
15.4141069240177));
#19207=CARTESIAN_POINT('Ctrl Pts',(-202.114952629401,-95.7324151709012,
15.5730152428221));
#19208=CARTESIAN_POINT('Ctrl Pts',(-202.821755867583,-92.9714120718513,
15.7319235616264));
#19209=CARTESIAN_POINT('Ctrl Pts',(-205.525536198956,-92.0702079824451,
15.8908318804307));
#19210=CARTESIAN_POINT('Ctrl Pts',(-207.747537243057,-93.8549791002543,
16.049740199235));
#19211=CARTESIAN_POINT('Ctrl Pts',(-207.450572215136,-96.6895450314807,
16.2086485180393));
#19212=CARTESIAN_POINT('Ctrl Pts',(-204.907062930782,-97.9750465199132,
16.3675568368436));
#19213=CARTESIAN_POINT('Ctrl Pts',(-202.44852376407,-96.5332828104831,16.5264651556479));
#19214=CARTESIAN_POINT('Ctrl Pts',(-202.329632350016,-93.68535893981,16.6853734744522));
#19215=CARTESIAN_POINT('Ctrl Pts',(-204.657905597619,-92.0436411981644,
16.8442817932565));
#19216=CARTESIAN_POINT('Ctrl Pts',(-207.301870908767,-93.1102820519823,
17.0031901120608));
#19217=CARTESIAN_POINT('Ctrl Pts',(-207.831183367532,-95.9134396039801,
17.1620984308651));
#19218=CARTESIAN_POINT('Ctrl Pts',(-206.459639356019,-97.2156893163364,
17.268037310068));
#19219=CARTESIAN_POINT('Ctrl Pts',(-205.650199997975,-97.4320868020351,
17.3210067496694));
#19220=CARTESIAN_POINT('Ctrl Pts',(-207.054331550342,-93.2435746787732,
-0.107002249889811));
#19221=CARTESIAN_POINT('Ctrl Pts',(-207.63889941333,-93.9272907410154,-0.0540328102883751));
#19222=CARTESIAN_POINT('Ctrl Pts',(-208.060448869472,-95.9135763642526,
0.051906068914496));
#19223=CARTESIAN_POINT('Ctrl Pts',(-205.887411436318,-98.0718309750383,
0.210814387718803));
#19224=CARTESIAN_POINT('Ctrl Pts',(-202.899439531812,-97.4076577124765,
0.36972270652311));
#19225=CARTESIAN_POINT('Ctrl Pts',(-201.83784878766,-94.5391936853839,0.528631025327416));
#19226=CARTESIAN_POINT('Ctrl Pts',(-203.674981979354,-92.0917369544157,
0.687539344131723));
#19227=CARTESIAN_POINT('Ctrl Pts',(-206.727022155188,-92.311247119458,0.84644766293603));
#19228=CARTESIAN_POINT('Ctrl Pts',(-208.195677430151,-94.9954354773421,
1.00535598174034));
#19229=CARTESIAN_POINT('Ctrl Pts',(-206.734605351153,-97.6839731807802,
1.16426430054464));
#19230=CARTESIAN_POINT('Ctrl Pts',(-203.683250030151,-97.911794637316,1.32317261934895));
#19231=CARTESIAN_POINT('Ctrl Pts',(-201.839084317695,-95.4701538312867,
1.48208093815326));
#19232=CARTESIAN_POINT('Ctrl Pts',(-202.892806927105,-92.5974626181698,
1.64098925695756));
#19233=CARTESIAN_POINT('Ctrl Pts',(-205.878382454666,-91.9273998345941,
1.79989757576187));
#19234=CARTESIAN_POINT('Ctrl Pts',(-208.058665865373,-94.0742581826815,
1.95880589456618));
#19235=CARTESIAN_POINT('Ctrl Pts',(-207.434799032048,-97.0698283899918,
2.11771421337048));
#19236=CARTESIAN_POINT('Ctrl Pts',(-204.57873544886,-98.1678020438509,2.27662253217479));
#19237=CARTESIAN_POINT('Ctrl Pts',(-202.108882599597,-96.361570682906,2.4355308509791));
#19238=CARTESIAN_POINT('Ctrl Pts',(-202.289573820351,-93.3070662993528,
2.5944391697834));
#19239=CARTESIAN_POINT('Ctrl Pts',(-204.955153492556,-91.8046247263461,
2.75334748858771));
#19240=CARTESIAN_POINT('Ctrl Pts',(-207.661847930024,-93.2316674343784,
2.91225580739202));
#19241=CARTESIAN_POINT('Ctrl Pts',(-207.928189941742,-96.2798977012732,
3.07116412619632));
#19242=CARTESIAN_POINT('Ctrl Pts',(-205.51000013995,-98.1547320477393,3.23007244500063));
#19243=CARTESIAN_POINT('Ctrl Pts',(-202.624247911321,-97.1373433189395,
3.38898076380494));
#19244=CARTESIAN_POINT('Ctrl Pts',(-201.916558643673,-94.1604621209265,
3.54788908260924));
#19245=CARTESIAN_POINT('Ctrl Pts',(-204.035733948823,-91.9532598685839,
3.70679740141355));
#19246=CARTESIAN_POINT('Ctrl Pts',(-207.038937592143,-92.5392749152246,
3.86570572021786));
#19247=CARTESIAN_POINT('Ctrl Pts',(-208.172866039841,-95.3812552169174,
4.02461403902216));
#19248=CARTESIAN_POINT('Ctrl Pts',(-206.397946364646,-97.8737049967838,
4.18352235782647));
#19249=CARTESIAN_POINT('Ctrl Pts',(-203.341405086918,-97.7315741544865,
4.34243067663077));
#19250=CARTESIAN_POINT('Ctrl Pts',(-201.805445087723,-95.0851666575561,
4.50133899543508));
#19251=CARTESIAN_POINT('Ctrl Pts',(-203.198217327227,-92.3606793208876,
4.66024731423939));
#19252=CARTESIAN_POINT('Ctrl Pts',(-206.242843782976,-92.0558916836784,
4.8191556330437));
#19253=CARTESIAN_POINT('Ctrl Pts',(-208.148044949501,-94.4502296451874,
4.978063951848));
#19254=CARTESIAN_POINT('Ctrl Pts',(-207.16715369137,-97.3485909233169,5.13697227065231));
#19255=CARTESIAN_POINT('Ctrl Pts',(-204.199440150821,-98.0937902926655,
5.29588058945661));
#19256=CARTESIAN_POINT('Ctrl Pts',(-201.965670932306,-96.0026373003525,
5.45478890826093));
#19257=CARTESIAN_POINT('Ctrl Pts',(-202.513740688985,-92.9922776373462,
5.61369722706523));
#19258=CARTESIAN_POINT('Ctrl Pts',(-205.341185193596,-91.8225753965231,
5.77260554586954));
#19259=CARTESIAN_POINT('Ctrl Pts',(-207.855834926075,-93.5659005187498,
5.93151386467385));
#19260=CARTESIAN_POINT('Ctrl Pts',(-207.752287117404,-96.6239920167532,
6.09042218347815));
#19261=CARTESIAN_POINT('Ctrl Pts',(-205.125473241242,-98.1932257848202,
6.24933050228246));
#19262=CARTESIAN_POINT('Ctrl Pts',(-202.383626899898,-96.8349458433886,
6.40823882108676));
#19263=CARTESIAN_POINT('Ctrl Pts',(-202.040442174065,-93.7944080615484,
6.56714713989107));
#19264=CARTESIAN_POINT('Ctrl Pts',(-204.410546984685,-91.8591434942289,
6.72605545869538));
#19265=CARTESIAN_POINT('Ctrl Pts',(-207.32105573155,-92.8033810666965,6.88496377749969));
#19266=CARTESIAN_POINT('Ctrl Pts',(-208.103646525691,-95.7614543260611,
7.04387209630399));
#19267=CARTESIAN_POINT('Ctrl Pts',(-206.040848873893,-98.0214347699103,
7.20278041510829));
#19268=CARTESIAN_POINT('Ctrl Pts',(-203.023812607864,-97.5113975866576,
7.36168873391261));
#19269=CARTESIAN_POINT('Ctrl Pts',(-201.818522855506,-94.6989391653287,
7.52059705271691));
#19270=CARTESIAN_POINT('Ctrl Pts',(-203.529975790509,-92.1624899523317,
7.67950537152122));
#19271=CARTESIAN_POINT('Ctrl Pts',(-206.589130490616,-92.2274382367739,
7.83841369032553));
#19272=CARTESIAN_POINT('Ctrl Pts',(-208.19138811831,-94.8342401573922,7.99732200912983));
#19273=CARTESIAN_POINT('Ctrl Pts',(-206.867816788622,-97.5930088490497,
8.15623032793414));
#19274=CARTESIAN_POINT('Ctrl Pts',(-203.831851903328,-97.9745360094224,
8.31513864673845));
#19275=CARTESIAN_POINT('Ctrl Pts',(-201.866832136913,-95.6290418021305,
8.47404696554275));
#19276=CARTESIAN_POINT('Ctrl Pts',(-202.774265648607,-92.7068491013155,
8.63295528434706));
#19277=CARTESIAN_POINT('Ctrl Pts',(-205.722227537085,-91.8869915143411,
8.79186360315137));
#19278=CARTESIAN_POINT('Ctrl Pts',(-208.008059291752,-93.9211053135663,
8.95077192195567));
#19279=CARTESIAN_POINT('Ctrl Pts',(-207.536135908197,-96.9443377027313,
9.10968024075998));
#19280=CARTESIAN_POINT('Ctrl Pts',(-204.739111469874,-98.1850230174926,
9.26858855956428));
#19281=CARTESIAN_POINT('Ctrl Pts',(-202.181266720073,-96.5057148281605,
9.4274968783686));
#19282=CARTESIAN_POINT('Ctrl Pts',(-202.20760513691,-93.4459841134342,9.58640519717289));
#19283=CARTESIAN_POINT('Ctrl Pts',(-204.793979954208,-91.8109577945972,
9.74531351597721));
#19284=CARTESIAN_POINT('Ctrl Pts',(-207.569231646844,-93.099609726408,9.90422183478151));
#19285=CARTESIAN_POINT('Ctrl Pts',(-207.989040481425,-96.1305182207789,
10.0631301535858));
#19286=CARTESIAN_POINT('Ctrl Pts',(-205.668530410522,-98.1249802459081,
10.2220384723901));
#19287=CARTESIAN_POINT('Ctrl Pts',(-202.735119131279,-97.2544953088468,
10.3809467911944));
#19288=CARTESIAN_POINT('Ctrl Pts',(-201.878125318374,-94.3171142706628,
10.5398551099987));
#19289=CARTESIAN_POINT('Ctrl Pts',(-203.883231321036,-92.0057952366625,
10.698763428803));
#19290=CARTESIAN_POINT('Ctrl Pts',(-206.912178366679,-92.4395296640824,
10.8576717476074));
#19291=CARTESIAN_POINT('Ctrl Pts',(-208.188061657773,-95.2206746776241,
11.0165800664117));
#19292=CARTESIAN_POINT('Ctrl Pts',(-206.541165653327,-97.7995076131551,
11.175488385216));
#19293=CARTESIAN_POINT('Ctrl Pts',(-203.481346203201,-97.8117832584635,
11.3343967040203));
#19294=CARTESIAN_POINT('Ctrl Pts',(-201.8138115803,-95.2462474391325,11.4933050228246));
#19295=CARTESIAN_POINT('Ctrl Pts',(-203.067338889211,-92.4549547198617,
11.6522133416289));
#19296=CARTESIAN_POINT('Ctrl Pts',(-206.09270830354,-91.9969310679766,11.8111216604332));
#19297=CARTESIAN_POINT('Ctrl Pts',(-208.116294958158,-94.2920874482903,
11.9700299792375));
#19298=CARTESIAN_POINT('Ctrl Pts',(-207.282897225321,-97.2362501438185,
12.1289382980418));
#19299=CARTESIAN_POINT('Ctrl Pts',(-204.356564831779,-98.1302437016009,
12.2878466168461));
#19300=CARTESIAN_POINT('Ctrl Pts',(-202.020126608923,-96.1544648198391,
12.4467549356504));
#19301=CARTESIAN_POINT('Ctrl Pts',(-202.415603005571,-93.1202854944699,
12.6056632544547));
#19302=CARTESIAN_POINT('Ctrl Pts',(-205.180425681454,-91.8094074185768,
12.764571573259));
#19303=CARTESIAN_POINT('Ctrl Pts',(-207.779836109132,-93.4236289607667,
12.9234798920633));
#19304=CARTESIAN_POINT('Ctrl Pts',(-207.83072386167,-96.4830498528951,13.0823882108676));
#19305=CARTESIAN_POINT('Ctrl Pts',(-205.286435616122,-98.1828272157492,
13.241296529672));
#19306=CARTESIAN_POINT('Ctrl Pts',(-202.479546399398,-96.9646241607618,
13.4002048484762));
#19307=CARTESIAN_POINT('Ctrl Pts',(-201.983380872592,-93.9452756338911,
13.5591131672806));
#19308=CARTESIAN_POINT('Ctrl Pts',(-204.252818046752,-91.8928866163885,
13.7180214860849));
#19309=CARTESIAN_POINT('Ctrl Pts',(-207.207263282303,-92.6890644235765,
13.8769298048892));
#19310=CARTESIAN_POINT('Ctrl Pts',(-208.138114215414,-95.6038821339156,
14.0358381236935));
#19311=CARTESIAN_POINT('Ctrl Pts',(-206.191977100272,-97.9650674625775,
14.1947464424978));
#19312=CARTESIAN_POINT('Ctrl Pts',(-203.153048721962,-97.6079120624099,
14.3536547613021));
#19313=CARTESIAN_POINT('Ctrl Pts',(-201.807384591263,-94.8598520709758,
14.5125630801064));
#19314=CARTESIAN_POINT('Ctrl Pts',(-203.388674669069,-92.2402780528891,
14.6714713989107));
#19315=CARTESIAN_POINT('Ctrl Pts',(-206.447209625131,-92.1507864397344,
14.830379717715));
#19316=CARTESIAN_POINT('Ctrl Pts',(-208.17895933528,-94.6734216248493,14.9892880365193));
#19317=CARTESIAN_POINT('Ctrl Pts',(-206.996273906404,-97.4954609351664,
15.1481963553236));
#19318=CARTESIAN_POINT('Ctrl Pts',(-203.9834284248,-98.0296880607766,15.3071046741279));
#19319=CARTESIAN_POINT('Ctrl Pts',(-201.902561191062,-95.7863341162865,
15.4660129929323));
#19320=CARTESIAN_POINT('Ctrl Pts',(-202.66139787518,-92.8220714709839,15.6249213117365));
#19321=CARTESIAN_POINT('Ctrl Pts',(-205.564225126678,-91.8545225323609,
15.7838296305409));
#19322=CARTESIAN_POINT('Ctrl Pts',(-207.949805459824,-93.7706849433184,
15.9427379493452));
#19323=CARTESIAN_POINT('Ctrl Pts',(-207.630978458316,-96.813925969912,16.1016462681495));
#19324=CARTESIAN_POINT('Ctrl Pts',(-204.900221088943,-98.1940635162815,
16.2605545869538));
#19325=CARTESIAN_POINT('Ctrl Pts',(-202.260689167953,-96.6461600355912,
16.4194629057581));
#19326=CARTESIAN_POINT('Ctrl Pts',(-202.133045204913,-93.5885776846673,
16.5783712245624));
#19327=CARTESIAN_POINT('Ctrl Pts',(-204.632721289413,-91.8259999543616,
16.7372795433667));
#19328=CARTESIAN_POINT('Ctrl Pts',(-207.471330058092,-92.9711647823235,
16.896187862171));
#19329=CARTESIAN_POINT('Ctrl Pts',(-208.039609445301,-95.9806852073979,
17.0550961809753));
#19330=CARTESIAN_POINT('Ctrl Pts',(-206.56709509676,-97.3788039485619,17.1610350601782));
#19331=CARTESIAN_POINT('Ctrl Pts',(-205.698066426161,-97.6111321859386,
17.2140044997796));
#19332=CARTESIAN_POINT('Ctrl Pts',(-207.195197104019,-93.1231365609213,
-0.214004499779621));
#19333=CARTESIAN_POINT('Ctrl Pts',(-207.819848796546,-93.8537350466211,
-0.161035060178185));
#19334=CARTESIAN_POINT('Ctrl Pts',(-208.270303906954,-95.9762203130131,
-0.0550961809753145));
#19335=CARTESIAN_POINT('Ctrl Pts',(-205.948261255469,-98.2824664837171,
0.103812137828992));
#19336=CARTESIAN_POINT('Ctrl Pts',(-202.755404060354,-97.5727508478452,
0.262720456633299));
#19337=CARTESIAN_POINT('Ctrl Pts',(-201.621020018583,-94.5075961875819,
0.421628775437606));
#19338=CARTESIAN_POINT('Ctrl Pts',(-203.584125468349,-91.8923173017865,
0.580537094241912));
#19339=CARTESIAN_POINT('Ctrl Pts',(-206.845444097382,-92.1268792830416,
0.739445413046219));
#19340=CARTESIAN_POINT('Ctrl Pts',(-208.414805092624,-94.9951224879363,
0.898353731850525));
#19341=CARTESIAN_POINT('Ctrl Pts',(-206.85354727324,-97.8680132730923,1.05726205065483));
#19342=CARTESIAN_POINT('Ctrl Pts',(-203.592960459548,-98.111456451258,1.21617036945914));
#19343=CARTESIAN_POINT('Ctrl Pts',(-201.622340268936,-95.5023922884853,
1.37507868826345));
#19344=CARTESIAN_POINT('Ctrl Pts',(-202.748316657816,-92.4327205839714,
1.53398700706775));
#19345=CARTESIAN_POINT('Ctrl Pts',(-205.938613156373,-91.7167115825171,
1.69289532587206));
#19346=CARTESIAN_POINT('Ctrl Pts',(-208.26839864223,-94.0107800485717,1.85180364467637));
#19347=CARTESIAN_POINT('Ctrl Pts',(-207.601753248218,-97.2117565622599,
2.01071196348067));
#19348=CARTESIAN_POINT('Ctrl Pts',(-204.549849330536,-98.3850182905525,
2.16962028228498));
#19349=CARTESIAN_POINT('Ctrl Pts',(-201.910638624185,-96.4549336106603,
2.32852860108929));
#19350=CARTESIAN_POINT('Ctrl Pts',(-202.103719845401,-93.1909818031377,
2.48743691989359));
#19351=CARTESIAN_POINT('Ctrl Pts',(-204.952078366683,-91.5855177827496,
2.6463452386979));
#19352=CARTESIAN_POINT('Ctrl Pts',(-207.844370893469,-93.1104128365508,
2.80525355750221));
#19353=CARTESIAN_POINT('Ctrl Pts',(-208.128975982022,-96.3676603111157,
2.96416187630651));
#19354=CARTESIAN_POINT('Ctrl Pts',(-205.544970859296,-98.3710520845579,
3.12307019511082));
#19355=CARTESIAN_POINT('Ctrl Pts',(-202.461342545186,-97.283900991176,3.28197851391513));
#19356=CARTESIAN_POINT('Ctrl Pts',(-201.705127010927,-94.1028949925101,
3.44088683271943));
#19357=CARTESIAN_POINT('Ctrl Pts',(-203.969614207261,-91.744344839532,3.59979515152374));
#19358=CARTESIAN_POINT('Ctrl Pts',(-207.178747581812,-92.370542949123,3.75870347032805));
#19359=CARTESIAN_POINT('Ctrl Pts',(-208.390429524845,-95.4073978944294,
3.91761178913235));
#19360=CARTESIAN_POINT('Ctrl Pts',(-206.493803573593,-98.0707550033463,
4.07652010793666));
#19361=CARTESIAN_POINT('Ctrl Pts',(-203.227675202022,-97.9188782464756,
4.23542842674096));
#19362=CARTESIAN_POINT('Ctrl Pts',(-201.586394396321,-95.0910065368929,
4.39433674554527));
#19363=CARTESIAN_POINT('Ctrl Pts',(-203.074669054913,-92.1797010514681,
4.55324506434958));
#19364=CARTESIAN_POINT('Ctrl Pts',(-206.328065604933,-91.8540141201495,
4.71215338315389));
#19365=CARTESIAN_POINT('Ctrl Pts',(-208.363906451865,-94.4125318814486,
4.87106170195819));
#19366=CARTESIAN_POINT('Ctrl Pts',(-207.315755461415,-97.5096338478239,
5.0299700207625));
#19367=CARTESIAN_POINT('Ctrl Pts',(-204.144545746659,-98.3059315521737,
5.1888783395668));
#19368=CARTESIAN_POINT('Ctrl Pts',(-201.757606930131,-96.0713881592039,
5.34778665837112));
#19369=CARTESIAN_POINT('Ctrl Pts',(-202.343257840502,-92.8546080765599,
5.50669497717542));
#19370=CARTESIAN_POINT('Ctrl Pts',(-205.364580268843,-91.6046993307239,
5.66560329597973));
#19371=CARTESIAN_POINT('Ctrl Pts',(-208.051659581547,-93.4675642899066,
5.82451161478403));
#19372=CARTESIAN_POINT('Ctrl Pts',(-207.941011497657,-96.7353491803859,
5.98341993358834));
#19373=CARTESIAN_POINT('Ctrl Pts',(-205.134076943793,-98.4121853379263,
6.14232825239264));
#19374=CARTESIAN_POINT('Ctrl Pts',(-202.204222146409,-96.9607681149461,
6.30123657119695));
#19375=CARTESIAN_POINT('Ctrl Pts',(-201.837505237367,-93.711740599283,6.46014489000126));
#19376=CARTESIAN_POINT('Ctrl Pts',(-204.370128180156,-91.6437749035884,
6.61905320880557));
#19377=CARTESIAN_POINT('Ctrl Pts',(-207.480210567431,-92.6527588644499,
6.77796152760988));
#19378=CARTESIAN_POINT('Ctrl Pts',(-208.316463627286,-95.8136672637549,
6.93686984641418));
#19379=CARTESIAN_POINT('Ctrl Pts',(-206.112219901073,-98.22861460984,7.09577816521849));
#19380=CARTESIAN_POINT('Ctrl Pts',(-202.888305400608,-97.683604167182,7.25468648402279));
#19381=CARTESIAN_POINT('Ctrl Pts',(-201.600368906892,-94.6782954181403,
7.4135948028271));
#19382=CARTESIAN_POINT('Ctrl Pts',(-203.429176202363,-91.967921834122,7.57250312163141));
#19383=CARTESIAN_POINT('Ctrl Pts',(-206.698097198735,-92.0373236236699,
7.73141144043571));
#19384=CARTESIAN_POINT('Ctrl Pts',(-208.410221662588,-94.8228740018159,
7.89031975924003));
#19385=CARTESIAN_POINT('Ctrl Pts',(-206.995893021523,-97.7708115153964,
8.04922807804432));
#19386=CARTESIAN_POINT('Ctrl Pts',(-203.751751966009,-98.178500000449,8.20813639684863));
#19387=CARTESIAN_POINT('Ctrl Pts',(-201.651990756648,-95.6721752105271,
8.36704471565293));
#19388=CARTESIAN_POINT('Ctrl Pts',(-202.621647001585,-92.5496077003575,
8.52595303445725));
#19389=CARTESIAN_POINT('Ctrl Pts',(-205.771750693109,-91.6735324629718,
8.68486135326155));
#19390=CARTESIAN_POINT('Ctrl Pts',(-208.214321974889,-93.8471254842938,
8.84376967206586));
#19391=CARTESIAN_POINT('Ctrl Pts',(-207.710038795902,-97.077660976175,9.00267799087017));
#19392=CARTESIAN_POINT('Ctrl Pts',(-204.721222338376,-98.4034201066862,
9.16158630967447));
#19393=CARTESIAN_POINT('Ctrl Pts',(-201.987986125186,-96.6089617227103,
9.32049462847878));
#19394=CARTESIAN_POINT('Ctrl Pts',(-202.016130567769,-93.3394252143862,
9.47940294728308));
#19395=CARTESIAN_POINT('Ctrl Pts',(-204.77985315573,-91.5922851096117,9.6383112660874));
#19396=CARTESIAN_POINT('Ctrl Pts',(-207.745403909981,-92.9692999290205,
9.7972195848917));
#19397=CARTESIAN_POINT('Ctrl Pts',(-208.193999044374,-96.2080378767884,
9.956127903696));
#19398=CARTESIAN_POINT('Ctrl Pts',(-205.714371553552,-98.3392602011063,
10.1150362225003));
#19399=CARTESIAN_POINT('Ctrl Pts',(-202.579816206816,-97.4090860952708,
10.2739445413046));
#19400=CARTESIAN_POINT('Ctrl Pts',(-201.664058311778,-94.2702887831483,
10.4328528601089));
#19401=CARTESIAN_POINT('Ctrl Pts',(-203.806654471371,-91.8004825588039,
10.5917611789132));
#19402=CARTESIAN_POINT('Ctrl Pts',(-207.043296473835,-92.2639581642033,
10.7506694977175));
#19403=CARTESIAN_POINT('Ctrl Pts',(-208.406667106589,-95.235806344487,10.9095778165218));
#19404=CARTESIAN_POINT('Ctrl Pts',(-206.646843411636,-97.991469903704,11.0684861353262));
#19405=CARTESIAN_POINT('Ctrl Pts',(-203.377212083324,-98.0045872902456,
11.2273944541305));
#19406=CARTESIAN_POINT('Ctrl Pts',(-201.595334579455,-95.2631326307411,
11.3863027729348));
#19407=CARTESIAN_POINT('Ctrl Pts',(-202.9348162799,-92.2804409163521,11.5452110917391));
#19408=CARTESIAN_POINT('Ctrl Pts',(-206.167635332802,-91.7910105739019,
11.7041194105434));
#19409=CARTESIAN_POINT('Ctrl Pts',(-208.329979363009,-94.2435458710873,
11.8630277293477));
#19410=CARTESIAN_POINT('Ctrl Pts',(-207.439435531701,-97.3895898589279,
12.021936048152));
#19411=CARTESIAN_POINT('Ctrl Pts',(-204.312444469995,-98.3448845720566,
12.1808443669563));
#19412=CARTESIAN_POINT('Ctrl Pts',(-201.815796633535,-96.233626494604,12.3397526857606));
#19413=CARTESIAN_POINT('Ctrl Pts',(-202.23839085426,-92.9913934348935,12.4986610045649));
#19414=CARTESIAN_POINT('Ctrl Pts',(-205.192797473881,-91.5906284242781,
12.6575693233692));
#19415=CARTESIAN_POINT('Ctrl Pts',(-207.970449524274,-93.3155371684729,
12.8164776421735));
#19416=CARTESIAN_POINT('Ctrl Pts',(-208.024826650977,-96.5847426096578,
12.9753859609778));
#19417=CARTESIAN_POINT('Ctrl Pts',(-205.306076511795,-98.4010737387753,
13.1342942797821));
#19418=CARTESIAN_POINT('Ctrl Pts',(-202.306718847825,-97.0993384770204,
13.2932025985864));
#19419=CARTESIAN_POINT('Ctrl Pts',(-201.77653124136,-93.8729531639453,13.4521109173908));
#19420=CARTESIAN_POINT('Ctrl Pts',(-204.201583765935,-91.6798317922794,
13.6110192361951));
#19421=CARTESIAN_POINT('Ctrl Pts',(-207.358615367764,-92.5306035269258,
13.7699275549994));
#19422=CARTESIAN_POINT('Ctrl Pts',(-208.353294767152,-95.6452903433819,
13.9288358738037));
#19423=CARTESIAN_POINT('Ctrl Pts',(-206.273710992823,-98.1683821951658,
14.087744192608));
#19424=CARTESIAN_POINT('Ctrl Pts',(-203.026403237521,-97.7867366423815,
14.2466525114123));
#19425=CARTESIAN_POINT('Ctrl Pts',(-201.588466891657,-94.8502421248036,
14.4055608302166));
#19426=CARTESIAN_POINT('Ctrl Pts',(-203.278186060326,-92.0510438662215,
14.5644691490209));
#19427=CARTESIAN_POINT('Ctrl Pts',(-206.546444816791,-91.9554158114422,
14.7233774678252));
#19428=CARTESIAN_POINT('Ctrl Pts',(-208.396940637668,-94.6510281394225,
14.8822857866295));
#19429=CARTESIAN_POINT('Ctrl Pts',(-207.133158446327,-97.6665747391933,
15.0411941054338));
#19430=CARTESIAN_POINT('Ctrl Pts',(-203.913722092456,-98.2374338290189,
15.2001024242381));
#19431=CARTESIAN_POINT('Ctrl Pts',(-201.690169752724,-95.8402530616716,
15.3590107430424));
#19432=CARTESIAN_POINT('Ctrl Pts',(-202.501039882777,-92.6727308701165,
15.5179190618467));
#19433=CARTESIAN_POINT('Ctrl Pts',(-205.6029140544,-91.6388370822767,15.6768273806511));
#19434=CARTESIAN_POINT('Ctrl Pts',(-208.152073676592,-93.6863907863824,
15.8357356994554));
#19435=CARTESIAN_POINT('Ctrl Pts',(-207.811384701495,-96.9383069083435,
15.9946440182597));
#19436=CARTESIAN_POINT('Ctrl Pts',(-204.893379247105,-98.4130805126498,
16.153552337064));
#19437=CARTESIAN_POINT('Ctrl Pts',(-202.072854571835,-96.7590372606993,
16.3124606558683));
#19438=CARTESIAN_POINT('Ctrl Pts',(-201.93645805981,-93.4917964295245,16.4713689746726));
#19439=CARTESIAN_POINT('Ctrl Pts',(-204.607536981208,-91.6083587105588,
16.6302772934769));
#19440=CARTESIAN_POINT('Ctrl Pts',(-207.640789207417,-92.8320475126647,
16.7891856122812));
#19441=CARTESIAN_POINT('Ctrl Pts',(-208.24803552307,-96.0479308108158,16.9480939310855));
#19442=CARTESIAN_POINT('Ctrl Pts',(-206.674550837501,-97.5419185807874,
17.0540328102884));
#19443=CARTESIAN_POINT('Ctrl Pts',(-205.745932854347,-97.7901775698422,
17.1070022498898));
#19444=CARTESIAN_POINT('Ctrl Pts',(-207.336062657696,-93.0026984430694,
-0.321006749669432));
#19445=CARTESIAN_POINT('Ctrl Pts',(-208.000798179763,-93.7801793522269,
-0.268037310067996));
#19446=CARTESIAN_POINT('Ctrl Pts',(-208.480158944437,-96.0388642617737,
-0.162098430865125));
#19447=CARTESIAN_POINT('Ctrl Pts',(-206.009111074621,-98.4931019923957,
-0.00319011206081841));
#19448=CARTESIAN_POINT('Ctrl Pts',(-202.611368588897,-97.7378439832139,
0.155718206743489));
#19449=CARTESIAN_POINT('Ctrl Pts',(-201.404191249506,-94.47599868978,0.314626525547795));
#19450=CARTESIAN_POINT('Ctrl Pts',(-203.493268957345,-91.692897649157,0.473534844352101));
#19451=CARTESIAN_POINT('Ctrl Pts',(-206.963866039577,-91.9425114466253,
0.632443163156408));
#19452=CARTESIAN_POINT('Ctrl Pts',(-208.633932755097,-94.9948094985304,
0.791351481960715));
#19453=CARTESIAN_POINT('Ctrl Pts',(-206.972489195327,-98.0520533654047,
0.950259800765021));
#19454=CARTESIAN_POINT('Ctrl Pts',(-203.502670888945,-98.3111182651998,
1.10916811956933));
#19455=CARTESIAN_POINT('Ctrl Pts',(-201.405596220178,-95.534630745684,1.26807643837364));
#19456=CARTESIAN_POINT('Ctrl Pts',(-202.603826388527,-92.2679785497729,
1.42698475717794));
#19457=CARTESIAN_POINT('Ctrl Pts',(-205.99884385808,-91.5060233304403,1.58589307598225));
#19458=CARTESIAN_POINT('Ctrl Pts',(-208.478131419088,-93.947301914462,1.74480139478656));
#19459=CARTESIAN_POINT('Ctrl Pts',(-207.768707464389,-97.3536847345279,
1.90370971359086));
#19460=CARTESIAN_POINT('Ctrl Pts',(-204.520963212211,-98.6022345372543,
2.06261803239517));
#19461=CARTESIAN_POINT('Ctrl Pts',(-201.712394648774,-96.5482965384147,
2.22152635119948));
#19462=CARTESIAN_POINT('Ctrl Pts',(-201.91786587045,-93.0748973069226,2.38043467000378));
#19463=CARTESIAN_POINT('Ctrl Pts',(-204.94900324081,-91.3664108391532,2.53934298880809));
#19464=CARTESIAN_POINT('Ctrl Pts',(-208.026893856913,-92.9891582387231,
2.6982513076124));
#19465=CARTESIAN_POINT('Ctrl Pts',(-208.329762022302,-96.4554229209582,
2.8571596264167));
#19466=CARTESIAN_POINT('Ctrl Pts',(-205.579941578641,-98.5873721213763,
3.01606794522101));
#19467=CARTESIAN_POINT('Ctrl Pts',(-202.298437179052,-97.4304586634127,
3.17497626402532));
#19468=CARTESIAN_POINT('Ctrl Pts',(-201.493695378181,-94.0453278640936,
3.33388458282962));
#19469=CARTESIAN_POINT('Ctrl Pts',(-203.9034944657,-91.5354298104801,3.49279290163393));
#19470=CARTESIAN_POINT('Ctrl Pts',(-207.318557571481,-92.2018109830213,
3.65170122043824));
#19471=CARTESIAN_POINT('Ctrl Pts',(-208.607993009848,-95.4335405719414,
3.81060953924254));
#19472=CARTESIAN_POINT('Ctrl Pts',(-206.589660782539,-98.2678050099089,
3.96951785804685));
#19473=CARTESIAN_POINT('Ctrl Pts',(-203.113945317127,-98.1061823384649,
4.12842617685115));
#19474=CARTESIAN_POINT('Ctrl Pts',(-201.36734370492,-95.0968464162294,4.28733449565546));
#19475=CARTESIAN_POINT('Ctrl Pts',(-202.951120782599,-91.9987227820489,
4.44624281445977));
#19476=CARTESIAN_POINT('Ctrl Pts',(-206.413287426889,-91.6521365566204,
4.60515113326408));
#19477=CARTESIAN_POINT('Ctrl Pts',(-208.57976795423,-94.3748341177099,4.76405945206838));
#19478=CARTESIAN_POINT('Ctrl Pts',(-207.464357231459,-97.6706767723307,
4.92296777087269));
#19479=CARTESIAN_POINT('Ctrl Pts',(-204.089651342497,-98.5180728116819,
5.081876089677));
#19480=CARTESIAN_POINT('Ctrl Pts',(-201.549542927956,-96.1401390180551,
5.2407844084813));
#19481=CARTESIAN_POINT('Ctrl Pts',(-202.172774992019,-92.7169385157737,
5.39969272728561));
#19482=CARTESIAN_POINT('Ctrl Pts',(-205.38797534409,-91.3868232649246,5.55860104608991));
#19483=CARTESIAN_POINT('Ctrl Pts',(-208.247484237019,-93.3692280610634,
5.71750936489423));
#19484=CARTESIAN_POINT('Ctrl Pts',(-208.129735877909,-96.8467063440184,
5.87641768369853));
#19485=CARTESIAN_POINT('Ctrl Pts',(-205.142680646343,-98.6311448910324,
6.03532600250284));
#19486=CARTESIAN_POINT('Ctrl Pts',(-202.024817392921,-97.0865903865035,
6.19423432130714));
#19487=CARTESIAN_POINT('Ctrl Pts',(-201.634568300669,-93.6290731370177,
6.35314264011145));
#19488=CARTESIAN_POINT('Ctrl Pts',(-204.329709375628,-91.4284063129477,
6.51205095891576));
#19489=CARTESIAN_POINT('Ctrl Pts',(-207.639365403312,-92.5021366622034,
6.67095927772007));
#19490=CARTESIAN_POINT('Ctrl Pts',(-208.529280728881,-95.8658802014486,
6.82986759652437));
#19491=CARTESIAN_POINT('Ctrl Pts',(-206.183590928253,-98.4357944497699,
6.98877591532868));
#19492=CARTESIAN_POINT('Ctrl Pts',(-202.752798193353,-97.8558107477063,
7.14768423413298));
#19493=CARTESIAN_POINT('Ctrl Pts',(-201.382214958278,-94.6576516709519,
7.30659255293729));
#19494=CARTESIAN_POINT('Ctrl Pts',(-203.328376614218,-91.7733537159122,
7.46550087174159));
#19495=CARTESIAN_POINT('Ctrl Pts',(-206.807063906854,-91.847209010566,7.62440919054591));
#19496=CARTESIAN_POINT('Ctrl Pts',(-208.629055206866,-94.8115078462396,
7.7833175093502));
#19497=CARTESIAN_POINT('Ctrl Pts',(-207.123969254423,-97.9486141817431,
7.94222582815452));
#19498=CARTESIAN_POINT('Ctrl Pts',(-203.67165202869,-98.3824639914755,8.10113414695881));
#19499=CARTESIAN_POINT('Ctrl Pts',(-201.437149376383,-95.715308618924,8.26004246576313));
#19500=CARTESIAN_POINT('Ctrl Pts',(-202.469028354564,-92.3923662993994,
8.41895078456744));
#19501=CARTESIAN_POINT('Ctrl Pts',(-205.821273849133,-91.4600734116028,
8.57785910337174));
#19502=CARTESIAN_POINT('Ctrl Pts',(-208.420584658025,-93.7731456550212,
8.73676742217605));
#19503=CARTESIAN_POINT('Ctrl Pts',(-207.883941683608,-97.2109842496187,
8.89567574098036));
#19504=CARTESIAN_POINT('Ctrl Pts',(-204.703333206878,-98.6218171958797,
9.05458405978466));
#19505=CARTESIAN_POINT('Ctrl Pts',(-201.7947055303,-96.7122086172601,9.21349237858897));
#19506=CARTESIAN_POINT('Ctrl Pts',(-201.824655998628,-93.2328663153382,
9.37240069739327));
#19507=CARTESIAN_POINT('Ctrl Pts',(-204.765726357252,-91.3736124246263,
9.53130901619759));
#19508=CARTESIAN_POINT('Ctrl Pts',(-207.921576173118,-92.8389901316329,
9.69021733500189));
#19509=CARTESIAN_POINT('Ctrl Pts',(-208.398957607323,-96.2855575327979,
9.84912565380619));
#19510=CARTESIAN_POINT('Ctrl Pts',(-205.76021269658,-98.5535401563045,10.0080339726105));
#19511=CARTESIAN_POINT('Ctrl Pts',(-202.424513282353,-97.5636768816949,
10.1669422914148));
#19512=CARTESIAN_POINT('Ctrl Pts',(-201.449991305182,-94.2234632956337,
10.3258506102191));
#19513=CARTESIAN_POINT('Ctrl Pts',(-203.730077621707,-91.5951698809454,
10.4847589290234));
#19514=CARTESIAN_POINT('Ctrl Pts',(-207.174414580991,-92.0883866643241,
10.6436672478277));
#19515=CARTESIAN_POINT('Ctrl Pts',(-208.625272555405,-95.2509380113502,
10.802575566632));
#19516=CARTESIAN_POINT('Ctrl Pts',(-206.752521169945,-98.1834321942526,
10.9614838854363));
#19517=CARTESIAN_POINT('Ctrl Pts',(-203.273077963447,-98.1973913220278,
11.1203922042406));
#19518=CARTESIAN_POINT('Ctrl Pts',(-201.37685757861,-95.2800178223495,11.279300523045));
#19519=CARTESIAN_POINT('Ctrl Pts',(-202.802293670589,-92.1059271128426,
11.4382088418493));
#19520=CARTESIAN_POINT('Ctrl Pts',(-206.242562362063,-91.5850900798271,
11.5971171606536));
#19521=CARTESIAN_POINT('Ctrl Pts',(-208.54366376786,-94.1950042938844,11.7560254794579));
#19522=CARTESIAN_POINT('Ctrl Pts',(-207.595973838081,-97.542929574037,11.9149337982622));
#19523=CARTESIAN_POINT('Ctrl Pts',(-204.26832410821,-98.5595254425124,12.0738421170665));
#19524=CARTESIAN_POINT('Ctrl Pts',(-201.611466658146,-96.3127881693687,
12.2327504358708));
#19525=CARTESIAN_POINT('Ctrl Pts',(-202.061178702949,-92.8625013753173,
12.3916587546751));
#19526=CARTESIAN_POINT('Ctrl Pts',(-205.205169266307,-91.3718494299793,
12.5505670734794));
#19527=CARTESIAN_POINT('Ctrl Pts',(-208.161062939416,-93.2074453761791,
12.7094753922837));
#19528=CARTESIAN_POINT('Ctrl Pts',(-208.218929440283,-96.6864353664204,
12.868383711088));
#19529=CARTESIAN_POINT('Ctrl Pts',(-205.325717407468,-98.6193202618013,
13.0272920298923));
#19530=CARTESIAN_POINT('Ctrl Pts',(-202.133891296251,-97.2340527932792,
13.1862003486966));
#19531=CARTESIAN_POINT('Ctrl Pts',(-201.569681610129,-93.8006306939993,
13.3451086675009));
#19532=CARTESIAN_POINT('Ctrl Pts',(-204.150349485118,-91.4667769681704,
13.5040169863052));
#19533=CARTESIAN_POINT('Ctrl Pts',(-207.509967453225,-92.3721426302753,
13.6629253051096));
#19534=CARTESIAN_POINT('Ctrl Pts',(-208.568475318891,-95.6866985528482,
13.8218336239139));
#19535=CARTESIAN_POINT('Ctrl Pts',(-206.355444885374,-98.3716969277542,
13.9807419427182));
#19536=CARTESIAN_POINT('Ctrl Pts',(-202.89975775308,-97.9655612223532,14.1396502615225));
#19537=CARTESIAN_POINT('Ctrl Pts',(-201.36954919205,-94.8406321786314,14.2985585803268));
#19538=CARTESIAN_POINT('Ctrl Pts',(-203.167697451582,-91.8618096795541,
14.4574668991311));
#19539=CARTESIAN_POINT('Ctrl Pts',(-206.64568000845,-91.7600451831499,14.6163752179354));
#19540=CARTESIAN_POINT('Ctrl Pts',(-208.614921940056,-94.6286346539956,
14.7752835367397));
#19541=CARTESIAN_POINT('Ctrl Pts',(-207.270042986249,-97.8376885432202,
14.934191855544));
#19542=CARTESIAN_POINT('Ctrl Pts',(-203.844015760112,-98.4451795972611,
15.0931001743483));
#19543=CARTESIAN_POINT('Ctrl Pts',(-201.477778314385,-95.8941720070566,
15.2520084931526));
#19544=CARTESIAN_POINT('Ctrl Pts',(-202.340681890374,-92.5233902692492,
15.4109168119569));
#19545=CARTESIAN_POINT('Ctrl Pts',(-205.641602982121,-91.4231516321926,
15.5698251307612));
#19546=CARTESIAN_POINT('Ctrl Pts',(-208.35434189336,-93.6020966294465,15.7287334495655));
#19547=CARTESIAN_POINT('Ctrl Pts',(-207.991790944675,-97.0626878467749,
15.8876417683698));
#19548=CARTESIAN_POINT('Ctrl Pts',(-204.886537405266,-98.6320975090182,
16.0465500871742));
#19549=CARTESIAN_POINT('Ctrl Pts',(-201.885019975718,-96.8719144858073,
16.2054584059785));
#19550=CARTESIAN_POINT('Ctrl Pts',(-201.739870914707,-93.3950151743818,
16.3643667247828));
#19551=CARTESIAN_POINT('Ctrl Pts',(-204.582352673002,-91.390717466756,16.5232750435871));
#19552=CARTESIAN_POINT('Ctrl Pts',(-207.810248356741,-92.6929302430059,
16.6821833623914));
#19553=CARTESIAN_POINT('Ctrl Pts',(-208.456461600838,-96.1151764142335,
16.8410916811957));
#19554=CARTESIAN_POINT('Ctrl Pts',(-206.782006578242,-97.7050332130129,
16.9470305603986));
#19555=CARTESIAN_POINT('Ctrl Pts',(-205.793799282533,-97.9692229537457,
17.));
#19556=CARTESIAN_POINT('Ctrl Pts',(-206.913465996665,-93.3640127966251,
0.));
#19557=CARTESIAN_POINT('Ctrl Pts',(-206.975062216132,-93.4218981178264,
-1.31381266890706E-17));
#19558=CARTESIAN_POINT('Ctrl Pts',(-207.033286091207,-93.482935106556,-1.69718597115089E-16));
#19559=CARTESIAN_POINT('Ctrl Pts',(-207.088141399968,-93.5467387008732,
-1.73472347597681E-16));
#19560=CARTESIAN_POINT('Ctrl Pts',(-207.144450725543,-93.6122334988504,
-1.77325596496041E-16));
#19561=CARTESIAN_POINT('Ctrl Pts',(-207.197210975624,-93.68064394337,-2.67124571148989E-16));
#19562=CARTESIAN_POINT('Ctrl Pts',(-207.246400666372,-93.7516020865845,
-2.15105711021124E-16));
#19563=CARTESIAN_POINT('Ctrl Pts',(-207.297350695962,-93.8250995906632,
-1.61225265293368E-16));
#19564=CARTESIAN_POINT('Ctrl Pts',(-207.34447062712,-93.9013309190617,2.27940104476882E-16));
#19565=CARTESIAN_POINT('Ctrl Pts',(-207.38770149442,-93.979931379362,2.35922392732846E-16));
#19566=CARTESIAN_POINT('Ctrl Pts',(-207.406614998863,-94.0143190807433,
2.3941464384483E-16));
#19567=CARTESIAN_POINT('Ctrl Pts',(-207.424783615686,-94.0491607575792,
3.42879087734196E-16));
#19568=CARTESIAN_POINT('Ctrl Pts',(-207.44219995004,-94.0844279691951,3.67761376907083E-16));
#19569=CARTESIAN_POINT('Ctrl Pts',(-207.451657071589,-94.1035781703914,
3.81272534213045E-16));
#19570=CARTESIAN_POINT('Ctrl Pts',(-207.460892353772,-94.122853861087,-1.08199995754127E-16));
#19571=CARTESIAN_POINT('Ctrl Pts',(-207.469904412035,-94.1422506144636,
-1.38777878078145E-16));
#19572=CARTESIAN_POINT('Ctrl Pts',(-207.478555202027,-94.1608698061163,
-1.68129978415293E-16));
#19573=CARTESIAN_POINT('Ctrl Pts',(-207.487002799098,-94.1796065572533,
2.27509235892531E-16));
#19574=CARTESIAN_POINT('Ctrl Pts',(-207.495231872231,-94.1984241373372,
1.94289029309402E-16));
#19575=CARTESIAN_POINT('Ctrl Pts',(-207.531772015166,-94.2819811862123,
4.6778966234489E-17));
#19576=CARTESIAN_POINT('Ctrl Pts',(-207.564052792852,-94.3672219361847,
1.51760739280742E-16));
#19577=CARTESIAN_POINT('Ctrl Pts',(-207.592050671291,-94.4537471119226,
4.16333634234434E-17));
#19578=CARTESIAN_POINT('Ctrl Pts',(-207.620513098777,-94.5417079388662,
-7.03212782969341E-17));
#19579=CARTESIAN_POINT('Ctrl Pts',(-207.64454981266,-94.6309969241772,-2.46766243899794E-16));
#19580=CARTESIAN_POINT('Ctrl Pts',(-207.664096969712,-94.7212317285697,
-3.05311331771918E-16));
#19581=CARTESIAN_POINT('Ctrl Pts',(-207.683346860096,-94.8100942720475,
-3.62966085405676E-16));
#19582=CARTESIAN_POINT('Ctrl Pts',(-207.698242981348,-94.8998749945991,
-1.93681199868498E-16));
#19583=CARTESIAN_POINT('Ctrl Pts',(-207.708681347609,-94.9902317459613,
-1.2490009027033E-16));
#19584=CARTESIAN_POINT('Ctrl Pts',(-207.712775191561,-95.025668942816,-9.79246879459923E-17));
#19585=CARTESIAN_POINT('Ctrl Pts',(-207.716182873916,-95.0611949208303,
-3.69133290614202E-16));
#19586=CARTESIAN_POINT('Ctrl Pts',(-207.718896131003,-95.0967895639108,
-4.02455846426619E-16));
#19587=CARTESIAN_POINT('Ctrl Pts',(-207.720491590831,-95.1177200623165,
-4.22050303371335E-16));
#19588=CARTESIAN_POINT('Ctrl Pts',(-207.721846915935,-95.1386743071217,
-2.20645000857552E-16));
#19589=CARTESIAN_POINT('Ctrl Pts',(-207.722960233087,-95.1596482300522,
-2.22044604925031E-16));
#19590=CARTESIAN_POINT('Ctrl Pts',(-207.723721698985,-95.1739935826248,
-2.2300188000784E-16));
#19591=CARTESIAN_POINT('Ctrl Pts',(-207.724369888774,-95.1883485234433,
-1.87428557882604E-16));
#19592=CARTESIAN_POINT('Ctrl Pts',(-207.724903817588,-95.2026963903353,
-1.94289029309402E-16));
#19593=CARTESIAN_POINT('Ctrl Pts',(-207.728446146415,-95.2978867251433,
-2.39804545795279E-16));
#19594=CARTESIAN_POINT('Ctrl Pts',(-207.726972459038,-95.3929268374015,
-1.01495799011983E-16));
#19595=CARTESIAN_POINT('Ctrl Pts',(-207.720424921853,-95.4874173617819,
-1.11022302462516E-16));
#19596=CARTESIAN_POINT('Ctrl Pts',(-207.713899316081,-95.5815913838534,
-1.2051689625484E-16));
#19597=CARTESIAN_POINT('Ctrl Pts',(-207.702334152436,-95.6752204482728,
-2.71226026961406E-16));
#19598=CARTESIAN_POINT('Ctrl Pts',(-207.685624183999,-95.7679271110661,
-2.77555756156289E-16));
#19599=CARTESIAN_POINT('Ctrl Pts',(-207.683541364687,-95.7794825624354,
-2.7834472725813E-16));
#19600=CARTESIAN_POINT('Ctrl Pts',(-207.681378547894,-95.7910236950498,
-6.25097225611804E-16));
#19601=CARTESIAN_POINT('Ctrl Pts',(-207.679135472956,-95.8025497860598,
-6.38378239159465E-16));
#19602=CARTESIAN_POINT('Ctrl Pts',(-207.661514670061,-95.8930946779994,
-7.71497736738381E-16));
#19603=CARTESIAN_POINT('Ctrl Pts',(-207.638945415372,-95.9827116524882,
-6.42240409036171E-16));
#19604=CARTESIAN_POINT('Ctrl Pts',(-207.611702718408,-96.0711633770076,
-6.93889390390723E-16));
#19605=CARTESIAN_POINT('Ctrl Pts',(-207.600775956761,-96.1066404412793,
-7.14605258182346E-16));
#19606=CARTESIAN_POINT('Ctrl Pts',(-207.589096771976,-96.1419299956307,
-4.97532461527305E-16));
#19607=CARTESIAN_POINT('Ctrl Pts',(-207.576680614638,-96.1770163619212,
-4.71844785465692E-16));
#19608=CARTESIAN_POINT('Ctrl Pts',(-207.570899237935,-96.1933537435407,
-4.59883747287457E-16));
#19609=CARTESIAN_POINT('Ctrl Pts',(-207.564958057168,-96.2096470667711,
2.78109615914965E-16));
#19610=CARTESIAN_POINT('Ctrl Pts',(-207.558858540981,-96.2258947231297,
3.05311331771918E-16));
#19611=CARTESIAN_POINT('Ctrl Pts',(-207.553795015448,-96.2393827474737,
3.27892890464571E-16));
#19612=CARTESIAN_POINT('Ctrl Pts',(-207.54862569686,-96.2528304121624,-4.55940524341242E-16));
#19613=CARTESIAN_POINT('Ctrl Pts',(-207.543352629307,-96.2662349571962,
-4.44089209850063E-16));
#19614=CARTESIAN_POINT('Ctrl Pts',(-207.509118978743,-96.3532595412822,
-3.67148462374673E-16));
#19615=CARTESIAN_POINT('Ctrl Pts',(-207.470506912078,-96.4384928583734,
9.67505829131724E-18));
#19616=CARTESIAN_POINT('Ctrl Pts',(-207.427848909633,-96.5217037647646,
-2.77555756156289E-17));
#19617=CARTESIAN_POINT('Ctrl Pts',(-207.38361239696,-96.6079937948706,-6.65712870024757E-17));
#19618=CARTESIAN_POINT('Ctrl Pts',(-207.33502484806,-96.6921096962562,-3.77517922847587E-16));
#19619=CARTESIAN_POINT('Ctrl Pts',(-207.28240107588,-96.7737901161264,-4.16333634234434E-16));
#19620=CARTESIAN_POINT('Ctrl Pts',(-207.229201427051,-96.8563643876647,
-4.55574116801746E-16));
#19621=CARTESIAN_POINT('Ctrl Pts',(-207.17187631397,-96.9364503981286,-2.0948851905607E-17));
#19622=CARTESIAN_POINT('Ctrl Pts',(-207.11069939243,-97.0137627199881,1.66533453693773E-16));
#19623=CARTESIAN_POINT('Ctrl Pts',(-207.08660648421,-97.0442101277357,2.40368387980402E-16));
#19624=CARTESIAN_POINT('Ctrl Pts',(-207.061915647846,-97.0742271107383,
-6.23795172114093E-17));
#19625=CARTESIAN_POINT('Ctrl Pts',(-207.036641661937,-97.1037951533782,
-5.55111512312578E-17));
#19626=CARTESIAN_POINT('Ctrl Pts',(-207.02229432359,-97.1205801082148,-5.16121710321849E-17));
#19627=CARTESIAN_POINT('Ctrl Pts',(-207.007759045441,-97.1372203785107,
-1.09560184887863E-16));
#19628=CARTESIAN_POINT('Ctrl Pts',(-206.993038388462,-97.1537124668965,
-1.11022302462516E-16));
#19629=CARTESIAN_POINT('Ctrl Pts',(-206.979026737747,-97.1694102297314,
-1.12413998552589E-16));
#19630=CARTESIAN_POINT('Ctrl Pts',(-206.964844314787,-97.1849766172826,
3.77293975944909E-17));
#19631=CARTESIAN_POINT('Ctrl Pts',(-206.9505123113,-97.2003885037202,2.77555756156289E-17));
#19632=CARTESIAN_POINT('Ctrl Pts',(-206.881794715978,-97.2742838091652,
-2.00658656184701E-17));
#19633=CARTESIAN_POINT('Ctrl Pts',(-206.80956588058,-97.3447172801099,-2.86357592693776E-16));
#19634=CARTESIAN_POINT('Ctrl Pts',(-206.734139318221,-97.4114022177255,
-3.33066907387547E-16));
#19635=CARTESIAN_POINT('Ctrl Pts',(-206.669026235039,-97.4689689654876,
-3.7338940648942E-16));
#19636=CARTESIAN_POINT('Ctrl Pts',(-206.601529082945,-97.5237422921457,
-1.64613334688922E-16));
#19637=CARTESIAN_POINT('Ctrl Pts',(-206.531822997772,-97.5755222055268,
-1.66533453693773E-16));
#19638=CARTESIAN_POINT('Ctrl Pts',(-206.504657943773,-97.5957012779787,
-1.67281740393871E-16));
#19639=CARTESIAN_POINT('Ctrl Pts',(-206.477157172808,-97.6154255432419,
-5.71199676364673E-16));
#19640=CARTESIAN_POINT('Ctrl Pts',(-206.449330183025,-97.6346823604932,
-5.55111512312578E-16));
#19641=CARTESIAN_POINT('Ctrl Pts',(-206.434059995963,-97.645249626444,-5.46283059200145E-16));
#19642=CARTESIAN_POINT('Ctrl Pts',(-206.418692843289,-97.6556751456101,
-2.60925414246822E-16));
#19643=CARTESIAN_POINT('Ctrl Pts',(-206.403240459967,-97.665950341847,-2.77555756156289E-16));
#19644=CARTESIAN_POINT('Ctrl Pts',(-206.316661269863,-97.723521924807,-3.70735009069288E-16));
#19645=CARTESIAN_POINT('Ctrl Pts',(-206.227325531817,-97.7764359916984,
-7.1156062831465E-16));
#19646=CARTESIAN_POINT('Ctrl Pts',(-206.135543110803,-97.8243696354571,
-5.55111512312578E-16));
#19647=CARTESIAN_POINT('Ctrl Pts',(-206.043760689789,-97.8723032792159,
-3.98662396310506E-16));
#19648=CARTESIAN_POINT('Ctrl Pts',(-205.949530933876,-97.9152574183469,
-6.03815084515193E-17));
#19649=CARTESIAN_POINT('Ctrl Pts',(-205.853125489076,-97.9528679072037,
1.11022302462516E-16));
#19650=CARTESIAN_POINT('Ctrl Pts',(-205.834025108086,-97.9603195056885,
1.44525943527419E-16));
#19651=CARTESIAN_POINT('Ctrl Pts',(-205.814839220958,-97.9675611910345,
-1.08059395429565E-16));
#19652=CARTESIAN_POINT('Ctrl Pts',(-205.795570948431,-97.974593906276,-1.11022302462516E-16));
#19653=CARTESIAN_POINT('Ctrl Pts',(-202.480282573446,-95.0019224211138,
1.61258330249195));
#19654=CARTESIAN_POINT('Ctrl Pts',(-202.479237170353,-95.125530122547,1.60474993100899));
#19655=CARTESIAN_POINT('Ctrl Pts',(-202.487545208479,-95.2489966935751,
1.59691655952602));
#19656=CARTESIAN_POINT('Ctrl Pts',(-202.505691710494,-95.3709998286824,
1.58908318804305));
#19657=CARTESIAN_POINT('Ctrl Pts',(-202.628398777888,-96.1959878571834,
1.53611374844161));
#19658=CARTESIAN_POINT('Ctrl Pts',(-203.200969189321,-96.9540603402788,
1.48314430884018));
#19659=CARTESIAN_POINT('Ctrl Pts',(-203.960941699756,-97.2977299593421,
1.43017486923874));
#19660=CARTESIAN_POINT('Ctrl Pts',(-204.720914210191,-97.6413995784054,
1.3772054296373));
#19661=CARTESIAN_POINT('Ctrl Pts',(-205.668288819629,-97.5706663334367,
1.32423599003587));
#19662=CARTESIAN_POINT('Ctrl Pts',(-206.368790514116,-97.1179356073323,
1.27126655043443));
#19663=CARTESIAN_POINT('Ctrl Pts',(-207.069292208603,-96.665204881228,1.218297110833));
#19664=CARTESIAN_POINT('Ctrl Pts',(-207.52292098814,-95.830476673988,1.16532767123156));
#19665=CARTESIAN_POINT('Ctrl Pts',(-207.521743785462,-94.9964236518891,
1.11235823163013));
#19666=CARTESIAN_POINT('Ctrl Pts',(-207.520566582783,-94.1623706297901,
1.05938879202869));
#19667=CARTESIAN_POINT('Ctrl Pts',(-207.064583397888,-93.3289927928321,
1.00641935242726));
#19668=CARTESIAN_POINT('Ctrl Pts',(-206.362798185001,-92.8782274828816,
0.95344991282582));
#19669=CARTESIAN_POINT('Ctrl Pts',(-205.661012972115,-92.4274621729311,
0.900480473224384));
#19670=CARTESIAN_POINT('Ctrl Pts',(-204.713425731236,-92.3593093899881,
0.847511033622949));
#19671=CARTESIAN_POINT('Ctrl Pts',(-203.95443862186,-92.70517209454,0.794541594021513));
#19672=CARTESIAN_POINT('Ctrl Pts',(-203.195451512484,-93.0510347990919,
0.741572154420077));
#19673=CARTESIAN_POINT('Ctrl Pts',(-202.625064534611,-93.8109129911388,
0.688602714818642));
#19674=CARTESIAN_POINT('Ctrl Pts',(-202.504670620096,-94.636147652816,0.635633275217206));
#19675=CARTESIAN_POINT('Ctrl Pts',(-202.487207239533,-94.7558496079226,
0.627949950975456));
#19676=CARTESIAN_POINT('Ctrl Pts',(-202.479211752923,-94.8769266689453,
0.620266626733705));
#19677=CARTESIAN_POINT('Ctrl Pts',(-202.480223490507,-94.9981350405341,
0.612583302491955));
#19678=CARTESIAN_POINT('Ctrl Pts',(-204.206200717467,-97.9692229537457,
-1.94289029309402E-15));
#19679=CARTESIAN_POINT('Ctrl Pts',(-203.217993421758,-97.7050332130129,
0.0529694396014337));
#19680=CARTESIAN_POINT('Ctrl Pts',(-201.543538352679,-96.1151767441382,
0.158908318804305));
#19681=CARTESIAN_POINT('Ctrl Pts',(-202.189751683364,-92.692930169225,0.317816637608612));
#19682=CARTESIAN_POINT('Ctrl Pts',(-205.417647323366,-91.3907175644162,
0.476724956412918));
#19683=CARTESIAN_POINT('Ctrl Pts',(-208.260129048284,-93.3950151579563,
0.635633275217225));
#19684=CARTESIAN_POINT('Ctrl Pts',(-208.114979996894,-96.8719144846003,
0.794541594021531));
#19685=CARTESIAN_POINT('Ctrl Pts',(-205.113462590801,-98.6320974631547,
0.953449912825839));
#19686=CARTESIAN_POINT('Ctrl Pts',(-202.00820908717,-97.0626878310035,1.11235823163014));
#19687=CARTESIAN_POINT('Ctrl Pts',(-201.645658139265,-93.6020966408935,
1.27126655043445));
#19688=CARTESIAN_POINT('Ctrl Pts',(-204.358397024947,-91.4231516694834,
1.43017486923876));
#19689=CARTESIAN_POINT('Ctrl Pts',(-207.659318082557,-92.523390293429,1.58908318804306));
#19690=CARTESIAN_POINT('Ctrl Pts',(-208.522221650421,-95.8941719984357,
1.74799150684737));
#19691=CARTESIAN_POINT('Ctrl Pts',(-206.155984228169,-98.445179562461,1.90689982565168));
#19692=CARTESIAN_POINT('Ctrl Pts',(-202.729957036615,-97.8376885148057,
2.06580814445599));
#19693=CARTESIAN_POINT('Ctrl Pts',(-201.385078096233,-94.628634657678,2.22471646326029));
#19694=CARTESIAN_POINT('Ctrl Pts',(-203.3543200081,-91.7600452157265,2.3836247820646));
#19695=CARTESIAN_POINT('Ctrl Pts',(-206.83230253,-91.8618097110707,2.5425331008689));
#19696=CARTESIAN_POINT('Ctrl Pts',(-208.630450771479,-94.8406321802388,
2.70144141967321));
#19697=CARTESIAN_POINT('Ctrl Pts',(-207.100242225817,-97.9655611925551,
2.86034973847752));
#19698=CARTESIAN_POINT('Ctrl Pts',(-203.644555128245,-98.3716968938806,
3.01925805728183));
#19699=CARTESIAN_POINT('Ctrl Pts',(-201.431524716961,-95.6866985459482,
3.17816637608613));
#19700=CARTESIAN_POINT('Ctrl Pts',(-202.490032571993,-92.3721426566775,
3.33707469489044));
#19701=CARTESIAN_POINT('Ctrl Pts',(-205.849650506345,-91.4667770036684,
3.49598301369474));
#19702=CARTESIAN_POINT('Ctrl Pts',(-208.430318355407,-93.8006307060494,
3.65489133249905));
#19703=CARTESIAN_POINT('Ctrl Pts',(-207.866108674953,-97.2340527708336,
3.81379965130336));
#19704=CARTESIAN_POINT('Ctrl Pts',(-204.674282595805,-98.6193202254382,
3.97270797010767));
#19705=CARTESIAN_POINT('Ctrl Pts',(-201.781070592057,-96.6864353494769,
4.13161628891197));
#19706=CARTESIAN_POINT('Ctrl Pts',(-201.838937092343,-93.2074453941888,
4.29052460771628));
#19707=CARTESIAN_POINT('Ctrl Pts',(-204.794830735755,-91.3718494664313,
4.44943292652058));
#19708=CARTESIAN_POINT('Ctrl Pts',(-207.938821267524,-92.8625013967925,
4.60834124532489));
#19709=CARTESIAN_POINT('Ctrl Pts',(-208.38853330781,-96.3127881561792,4.7672495641292));
#19710=CARTESIAN_POINT('Ctrl Pts',(-205.731675884439,-98.55952540675,4.92615788293351));
#19711=CARTESIAN_POINT('Ctrl Pts',(-202.404026188001,-97.5429295484884,
5.08506620173781));
#19712=CARTESIAN_POINT('Ctrl Pts',(-201.456336267743,-94.1950043019721,
5.24397452054212));
#19713=CARTESIAN_POINT('Ctrl Pts',(-203.75743765042,-91.5850901141365,5.40288283934643));
#19714=CARTESIAN_POINT('Ctrl Pts',(-207.19770630733,-92.1059271419192,5.56179115815073));
#19715=CARTESIAN_POINT('Ctrl Pts',(-208.623142384989,-95.2800178195362,
5.72069947695504));
#19716=CARTESIAN_POINT('Ctrl Pts',(-206.726922019203,-98.1973912899037,
5.87960779575934));
#19717=CARTESIAN_POINT('Ctrl Pts',(-203.247478847662,-98.1834321622689,
6.03851611456366));
#19718=CARTESIAN_POINT('Ctrl Pts',(-201.374727481018,-95.250938008829,6.19742443336796));
#19719=CARTESIAN_POINT('Ctrl Pts',(-202.825585440856,-92.088386693577,6.35633275217227));
#19720=CARTESIAN_POINT('Ctrl Pts',(-206.269922365534,-91.5951699151535,
6.51524107097657));
#19721=CARTESIAN_POINT('Ctrl Pts',(-208.550008659151,-94.2234633034355,
6.67414938978088));
#19722=CARTESIAN_POINT('Ctrl Pts',(-207.575486691771,-97.5636768559377,
6.83305770858518));
#19723=CARTESIAN_POINT('Ctrl Pts',(-204.239787311058,-98.5535401206023,
6.9919660273895));
#19724=CARTESIAN_POINT('Ctrl Pts',(-201.601042426826,-96.285557519882,7.1508743461938));
#19725=CARTESIAN_POINT('Ctrl Pts',(-202.078423856235,-92.8389901533445,
7.30978266499811));
#19726=CARTESIAN_POINT('Ctrl Pts',(-205.234273640395,-91.3736124610605,
7.46869098380241));
#19727=CARTESIAN_POINT('Ctrl Pts',(-208.175343969469,-93.2328663330924,
7.62759930260672));
#19728=CARTESIAN_POINT('Ctrl Pts',(-208.205294437497,-96.7122086000577,
7.78650762141102));
#19729=CARTESIAN_POINT('Ctrl Pts',(-205.296666790141,-98.6218171594914,
7.94541594021533));
#19730=CARTESIAN_POINT('Ctrl Pts',(-202.116058345367,-97.2109842274052,
8.10432425901964));
#19731=CARTESIAN_POINT('Ctrl Pts',(-201.579415376341,-93.7731456673473,
8.26323257782395));
#19732=CARTESIAN_POINT('Ctrl Pts',(-204.178726159118,-91.4600734471682,
8.42214089662825));
#19733=CARTESIAN_POINT('Ctrl Pts',(-207.530971620008,-92.3923663255981,
8.58104921543255));
#19734=CARTESIAN_POINT('Ctrl Pts',(-208.562850587821,-95.7153086117373,
8.73995753423687));
#19735=CARTESIAN_POINT('Ctrl Pts',(-206.328347957964,-98.382463957492,8.89886585304117));
#19736=CARTESIAN_POINT('Ctrl Pts',(-202.876030766917,-97.9486141521186,
9.05777417184548));
#19737=CARTESIAN_POINT('Ctrl Pts',(-201.370944829595,-94.8115078481334,
9.21668249064979));
#19738=CARTESIAN_POINT('Ctrl Pts',(-203.192936111301,-91.8472090422419,
9.3755908094541));
#19739=CARTESIAN_POINT('Ctrl Pts',(-206.671623368988,-91.7733537483301,
9.53449912825839));
#19740=CARTESIAN_POINT('Ctrl Pts',(-208.617785005374,-94.6576516743914,
9.69340744706271));
#19741=CARTESIAN_POINT('Ctrl Pts',(-207.247201784069,-97.8558107190141,
9.85231576586701));
#19742=CARTESIAN_POINT('Ctrl Pts',(-203.816409083639,-98.4357944152506,
10.0112240846713));
#19743=CARTESIAN_POINT('Ctrl Pts',(-201.470719306577,-95.8658801927493,
10.1701324034756));
#19744=CARTESIAN_POINT('Ctrl Pts',(-202.360634623205,-92.5021366872992,
10.3290407222799));
#19745=CARTESIAN_POINT('Ctrl Pts',(-205.670290617637,-91.4284063488314,
10.4879490410842));
#19746=CARTESIAN_POINT('Ctrl Pts',(-208.365431665519,-93.6290731507911,
10.6468573598885));
#19747=CARTESIAN_POINT('Ctrl Pts',(-207.975182577187,-97.0865903655397,
10.8057656786929));
#19748=CARTESIAN_POINT('Ctrl Pts',(-204.85731935509,-98.6311448545504,10.9646739974972));
#19749=CARTESIAN_POINT('Ctrl Pts',(-201.870264153535,-96.8467063254648,
11.1235823163015));
#19750=CARTESIAN_POINT('Ctrl Pts',(-201.752515795608,-93.3692280774477,
11.2824906351058));
#19751=CARTESIAN_POINT('Ctrl Pts',(-204.612024659808,-91.3868233012261,
11.4413989539101));
#19752=CARTESIAN_POINT('Ctrl Pts',(-207.827224979576,-92.7169385387114,
11.6003072727144));
#19753=CARTESIAN_POINT('Ctrl Pts',(-208.450457037378,-96.1401390066001,
11.7592155915187));
#19754=CARTESIAN_POINT('Ctrl Pts',(-205.910348648356,-98.5180727763361,
11.918123910323));
#19755=CARTESIAN_POINT('Ctrl Pts',(-202.5356427933,-97.6706767454985,12.0770322291273));
#19756=CARTESIAN_POINT('Ctrl Pts',(-201.420232081736,-94.374834123991,12.2359405479316));
#19757=CARTESIAN_POINT('Ctrl Pts',(-203.58671258731,-91.6521365902563,12.3948488667359));
#19758=CARTESIAN_POINT('Ctrl Pts',(-207.048879196816,-91.9987228122024,
12.5537571855402));
#19759=CARTESIAN_POINT('Ctrl Pts',(-208.632656258583,-95.0968464152565,
12.7126655043445));
#19760=CARTESIAN_POINT('Ctrl Pts',(-206.886054663924,-98.1061823072572,
12.8715738231488));
#19761=CARTESIAN_POINT('Ctrl Pts',(-203.410339233432,-98.2678049770775,
13.0304821419532));
#19762=CARTESIAN_POINT('Ctrl Pts',(-201.392007026401,-95.4335405675857,
13.1893904607575));
#19763=CARTESIAN_POINT('Ctrl Pts',(-202.681442451813,-92.2018110111346,
13.3482987795618));
#19764=CARTESIAN_POINT('Ctrl Pts',(-206.096505523284,-91.5354298452884,
13.5072070983661));
#19765=CARTESIAN_POINT('Ctrl Pts',(-208.506304586591,-94.045327873685,13.6661154171704));
#19766=CARTESIAN_POINT('Ctrl Pts',(-207.701562793806,-97.4304586389942,
13.8250237359747));
#19767=CARTESIAN_POINT('Ctrl Pts',(-204.420058427186,-98.5873720853337,
13.983932054779));
#19768=CARTESIAN_POINT('Ctrl Pts',(-201.670238011152,-96.4554229063367,
14.1428403735833));
#19769=CARTESIAN_POINT('Ctrl Pts',(-201.973106173498,-92.989158258924,14.3017486923876));
#19770=CARTESIAN_POINT('Ctrl Pts',(-205.050996758677,-91.3664108756636,
14.4606570111919));
#19771=CARTESIAN_POINT('Ctrl Pts',(-208.082134098584,-93.0748973262563,
14.6195653299962));
#19772=CARTESIAN_POINT('Ctrl Pts',(-208.287605318196,-96.548296522874,14.7784736488005));
#19773=CARTESIAN_POINT('Ctrl Pts',(-205.479036782975,-98.6022345010335,
14.9373819676048));
#19774=CARTESIAN_POINT('Ctrl Pts',(-202.231292563431,-97.3536847109377,
15.0962902864091));
#19775=CARTESIAN_POINT('Ctrl Pts',(-201.521868615849,-93.9473019249279,
15.2551986052134));
#19776=CARTESIAN_POINT('Ctrl Pts',(-204.001156151974,-91.5060233657571,
15.4141069240177));
#19777=CARTESIAN_POINT('Ctrl Pts',(-207.396173587353,-92.2679785768132,
15.5730152428221));
#19778=CARTESIAN_POINT('Ctrl Pts',(-208.594403743819,-95.5346307410897,
15.7319235616264));
#19779=CARTESIAN_POINT('Ctrl Pts',(-206.497329095757,-98.3111182304646,
15.8908318804307));
#19780=CARTESIAN_POINT('Ctrl Pts',(-203.027510825076,-98.0520533374907,
16.049740199235));
#19781=CARTESIAN_POINT('Ctrl Pts',(-201.36606728008,-94.9948094934893,16.2086485180393));
#19782=CARTESIAN_POINT('Ctrl Pts',(-203.036133983161,-91.9425114866494,
16.3675568368436));
#19783=CARTESIAN_POINT('Ctrl Pts',(-206.506731020769,-91.6928976656653,
16.5264651556479));
#19784=CARTESIAN_POINT('Ctrl Pts',(-208.595808729299,-94.4759987242795,
16.6853734744522));
#19785=CARTESIAN_POINT('Ctrl Pts',(-207.388631352792,-97.7378439047888,
16.8442817932565));
#19786=CARTESIAN_POINT('Ctrl Pts',(-203.990889000222,-98.4931020304819,
17.0031901120608));
#19787=CARTESIAN_POINT('Ctrl Pts',(-201.519840830385,-96.0388640162284,
17.1620984308651));
#19788=CARTESIAN_POINT('Ctrl Pts',(-201.999201820237,-93.780179352227,17.268037310068));
#19789=CARTESIAN_POINT('Ctrl Pts',(-202.663937342304,-93.0026984430694,
17.3210067496694));
#19790=CARTESIAN_POINT('Ctrl Pts',(-204.254067145653,-97.7901775698422,
-0.107002249889813));
#19791=CARTESIAN_POINT('Ctrl Pts',(-203.325449162499,-97.5419185807874,
-0.054032810288377));
#19792=CARTESIAN_POINT('Ctrl Pts',(-201.75196443325,-96.047931120827,0.0519060689144942));
#19793=CARTESIAN_POINT('Ctrl Pts',(-202.35921083027,-92.8320474433327,0.210814387718801));
#19794=CARTESIAN_POINT('Ctrl Pts',(-205.39246301538,-91.6083588023301,0.369722706523108));
#19795=CARTESIAN_POINT('Ctrl Pts',(-208.063541905413,-93.4917964140895,
0.528631025327414));
#19796=CARTESIAN_POINT('Ctrl Pts',(-207.927145402428,-96.7590372595651,
0.687539344131721));
#19797=CARTESIAN_POINT('Ctrl Pts',(-205.106620749199,-98.4130804695519,
0.846447662936027));
#19798=CARTESIAN_POINT('Ctrl Pts',(-202.18861532843,-96.9383068935231,1.00535598174034));
#19799=CARTESIAN_POINT('Ctrl Pts',(-201.847926354066,-93.686390797139,1.16426430054464));
#19800=CARTESIAN_POINT('Ctrl Pts',(-204.397085952243,-91.638837117319,1.32317261934895));
#19801=CARTESIAN_POINT('Ctrl Pts',(-207.498960091786,-92.6727308928383,
1.48208093815325));
#19802=CARTESIAN_POINT('Ctrl Pts',(-208.309830214205,-95.8402530535703,
1.64098925695756));
#19803=CARTESIAN_POINT('Ctrl Pts',(-206.086277896531,-98.2374337963173,
1.79989757576187));
#19804=CARTESIAN_POINT('Ctrl Pts',(-202.866841575158,-97.6665747124921,
1.95880589456617));
#19805=CARTESIAN_POINT('Ctrl Pts',(-201.603059396433,-94.6510281428828,
2.11771421337048));
#19806=CARTESIAN_POINT('Ctrl Pts',(-203.453555198761,-91.9554158420543,
2.27662253217479));
#19807=CARTESIAN_POINT('Ctrl Pts',(-206.721813922367,-92.0510438958378,
2.4355308509791));
#19808=CARTESIAN_POINT('Ctrl Pts',(-208.411533074072,-94.8502421263141,
2.5944391697834));
#19809=CARTESIAN_POINT('Ctrl Pts',(-206.973596742648,-97.7867366143803,
2.75334748858771));
#19810=CARTESIAN_POINT('Ctrl Pts',(-203.726289019975,-98.1683821633347,
2.91225580739202));
#19811=CARTESIAN_POINT('Ctrl Pts',(-201.646705266537,-95.645290336898,3.07116412619632));
#19812=CARTESIAN_POINT('Ctrl Pts',(-202.641384655933,-92.5306035517361,
3.23007244500063));
#19813=CARTESIAN_POINT('Ctrl Pts',(-205.798416226043,-91.6798318256369,
3.38898076380493));
#19814=CARTESIAN_POINT('Ctrl Pts',(-208.223468726254,-93.8729531752686,
3.54788908260924));
#19815=CARTESIAN_POINT('Ctrl Pts',(-207.693281125116,-97.0993384559284,
3.70679740141355));
#19816=CARTESIAN_POINT('Ctrl Pts',(-204.69392349128,-98.4010737046049,3.86570572021786));
#19817=CARTESIAN_POINT('Ctrl Pts',(-201.975173379413,-96.584742593736,4.02461403902216));
#19818=CARTESIAN_POINT('Ctrl Pts',(-202.02955050557,-93.3155371853966,4.18352235782647));
#19819=CARTESIAN_POINT('Ctrl Pts',(-204.807202528057,-91.5906284585319,
4.34243067663077));
#19820=CARTESIAN_POINT('Ctrl Pts',(-207.761609117994,-92.9913934550739,
4.50133899543508));
#19821=CARTESIAN_POINT('Ctrl Pts',(-208.184203334474,-96.2336264822096,
4.66024731423938));
#19822=CARTESIAN_POINT('Ctrl Pts',(-205.687555523098,-98.3448845384508,
4.8191556330437));
#19823=CARTESIAN_POINT('Ctrl Pts',(-202.560564492808,-97.3895898349197,
4.978063951848));
#19824=CARTESIAN_POINT('Ctrl Pts',(-201.670020670447,-94.2435458786875,
5.13697227065231));
#19825=CARTESIAN_POINT('Ctrl Pts',(-203.832364678929,-91.7910106061423,
5.29588058945662));
#19826=CARTESIAN_POINT('Ctrl Pts',(-207.065183699351,-92.2804409436754,
5.45478890826092));
#19827=CARTESIAN_POINT('Ctrl Pts',(-208.404665386339,-95.2631326280973,
5.61369722706523));
#19828=CARTESIAN_POINT('Ctrl Pts',(-206.622787900372,-98.0045872600586,
5.77260554586953));
#19829=CARTESIAN_POINT('Ctrl Pts',(-203.35315660491,-97.9914698736489,5.93151386467385));
#19830=CARTESIAN_POINT('Ctrl Pts',(-201.593332927638,-95.235806342118,6.09042218347814));
#19831=CARTESIAN_POINT('Ctrl Pts',(-202.956703546694,-92.2639581916921,
6.24933050228246));
#19832=CARTESIAN_POINT('Ctrl Pts',(-206.193345516639,-91.8004825909493,
6.40823882108676));
#19833=CARTESIAN_POINT('Ctrl Pts',(-208.335941654706,-94.2702887904795,
6.56714713989107));
#19834=CARTESIAN_POINT('Ctrl Pts',(-207.420183768868,-97.4090860710669,
6.72605545869537));
#19835=CARTESIAN_POINT('Ctrl Pts',(-204.285628453626,-98.3392601675569,
6.88496377749969));
#19836=CARTESIAN_POINT('Ctrl Pts',(-201.806000987716,-96.2080378646515,
7.04387209630398));
#19837=CARTESIAN_POINT('Ctrl Pts',(-202.254596117602,-92.9692999494227,
7.20278041510831));
#19838=CARTESIAN_POINT('Ctrl Pts',(-205.220146842058,-91.5922851438489,
7.36168873391259));
#19839=CARTESIAN_POINT('Ctrl Pts',(-207.983869402252,-93.3394252310698,
7.52059705271691));
#19840=CARTESIAN_POINT('Ctrl Pts',(-208.012013844552,-96.6089617065452,
7.67950537152121));
#19841=CARTESIAN_POINT('Ctrl Pts',(-205.278777658823,-98.4034200724921,
7.83841369032552));
#19842=CARTESIAN_POINT('Ctrl Pts',(-202.289961231325,-97.0776609553009,
7.99732200912983));
#19843=CARTESIAN_POINT('Ctrl Pts',(-201.785678057406,-93.8471254958766,
8.15623032793413));
#19844=CARTESIAN_POINT('Ctrl Pts',(-204.228249314645,-91.6735324963928,
8.31513864673845));
#19845=CARTESIAN_POINT('Ctrl Pts',(-207.37835297452,-92.5496077249763,8.47404696554274));
#19846=CARTESIAN_POINT('Ctrl Pts',(-208.348009209715,-95.6721752037739,
8.63295528434706));
#19847=CARTESIAN_POINT('Ctrl Pts',(-206.24824802145,-98.1784999685146,8.79186360315136));
#19848=CARTESIAN_POINT('Ctrl Pts',(-203.00410699853,-97.7708114875583,8.95077192195567));
#19849=CARTESIAN_POINT('Ctrl Pts',(-201.589778371674,-94.8228740035955,
9.10968024075998));
#19850=CARTESIAN_POINT('Ctrl Pts',(-203.301902818326,-92.0373236534358,
9.26858855956428));
#19851=CARTESIAN_POINT('Ctrl Pts',(-206.570823781855,-91.967921864585,9.42749687836858));
#19852=CARTESIAN_POINT('Ctrl Pts',(-208.399631058952,-94.6782954213725,
9.5864051971729));
#19853=CARTESIAN_POINT('Ctrl Pts',(-207.111694578176,-97.6836041402198,
9.7453135159772));
#19854=CARTESIAN_POINT('Ctrl Pts',(-203.887780110101,-98.2286145774026,
9.90422183478151));
#19855=CARTESIAN_POINT('Ctrl Pts',(-201.683536406035,-95.81366725558,10.0631301535858));
#19856=CARTESIAN_POINT('Ctrl Pts',(-202.519789457487,-92.6527588880325,
10.2220384723901));
#19857=CARTESIAN_POINT('Ctrl Pts',(-205.629871813515,-91.6437749373083,
10.3809467911944));
#19858=CARTESIAN_POINT('Ctrl Pts',(-208.162494730859,-93.7117406122259,
10.5398551099987));
#19859=CARTESIAN_POINT('Ctrl Pts',(-207.795777825502,-96.9607680952463,
10.698763428803));
#19860=CARTESIAN_POINT('Ctrl Pts',(-204.865923057554,-98.4121853036442,
10.8576717476073));
#19861=CARTESIAN_POINT('Ctrl Pts',(-202.058988531892,-96.735349162951,11.0165800664117));
#19862=CARTESIAN_POINT('Ctrl Pts',(-201.948340449113,-93.4675643053029,
11.175488385216));
#19863=CARTESIAN_POINT('Ctrl Pts',(-204.63541973482,-91.6046993648363,11.3343967040203));
#19864=CARTESIAN_POINT('Ctrl Pts',(-207.656742132806,-92.8546080981145,
11.4933050228246));
#19865=CARTESIAN_POINT('Ctrl Pts',(-208.242393037293,-96.0713881484396,
11.6522133416289));
#19866=CARTESIAN_POINT('Ctrl Pts',(-205.855454244746,-98.3059315189592,
11.8111216604332));
#19867=CARTESIAN_POINT('Ctrl Pts',(-202.684244561852,-97.5096338226097,
11.9700299792375));
#19868=CARTESIAN_POINT('Ctrl Pts',(-201.636093581931,-94.412531887351,12.1289382980418));
#19869=CARTESIAN_POINT('Ctrl Pts',(-203.671934408411,-91.854014151757,12.2878466168461));
#19870=CARTESIAN_POINT('Ctrl Pts',(-206.925330925743,-92.1797010798036,
12.4467549356504));
#19871=CARTESIAN_POINT('Ctrl Pts',(-208.413605569382,-95.0910065359784,
12.6056632544547));
#19872=CARTESIAN_POINT('Ctrl Pts',(-206.772324780171,-97.9188782171498,
12.764571573259));
#19873=CARTESIAN_POINT('Ctrl Pts',(-203.506196441416,-98.0707549724947,
12.9234798920633));
#19874=CARTESIAN_POINT('Ctrl Pts',(-201.609570509219,-95.4073978903364,
13.0823882108676));
#19875=CARTESIAN_POINT('Ctrl Pts',(-202.821252440078,-92.3705429755409,
13.241296529672));
#19876=CARTESIAN_POINT('Ctrl Pts',(-206.030385782386,-91.7443448722414,
13.4002048484763));
#19877=CARTESIAN_POINT('Ctrl Pts',(-208.29487295597,-94.1028950015231,13.5591131672806));
#19878=CARTESIAN_POINT('Ctrl Pts',(-207.538657429308,-97.28390096823,13.7180214860849));
#19879=CARTESIAN_POINT('Ctrl Pts',(-204.45502914618,-98.3710520506886,13.8769298048892));
#19880=CARTESIAN_POINT('Ctrl Pts',(-201.871024049414,-96.3676602973758,
14.0358381236935));
#19881=CARTESIAN_POINT('Ctrl Pts',(-202.155629135109,-93.1104128555335,
14.1947464424978));
#19882=CARTESIAN_POINT('Ctrl Pts',(-205.047921632835,-91.5855178170584,
14.3536547613021));
#19883=CARTESIAN_POINT('Ctrl Pts',(-207.896280125501,-93.1909818213055,
14.5125630801064));
#19884=CARTESIAN_POINT('Ctrl Pts',(-208.089361344776,-96.4549335960568,
14.6714713989107));
#19885=CARTESIAN_POINT('Ctrl Pts',(-205.450150664941,-98.3850182565158,
14.830379717715));
#19886=CARTESIAN_POINT('Ctrl Pts',(-202.398246777924,-97.2117565400922,
14.9892880365193));
#19887=CARTESIAN_POINT('Ctrl Pts',(-201.7316013906,-94.0107800584065,15.1481963553236));
#19888=CARTESIAN_POINT('Ctrl Pts',(-204.061386853075,-91.7167116157045,
15.3071046741279));
#19889=CARTESIAN_POINT('Ctrl Pts',(-207.251683319518,-92.4327206093809,
15.4660129929323));
#19890=CARTESIAN_POINT('Ctrl Pts',(-208.377659697231,-95.5023922841682,
15.6249213117365));
#19891=CARTESIAN_POINT('Ctrl Pts',(-206.407039526077,-98.1114564186172,
15.7838296305409));
#19892=CARTESIAN_POINT('Ctrl Pts',(-203.146452745933,-97.8680132468618,
15.9427379493452));
#19893=CARTESIAN_POINT('Ctrl Pts',(-201.585194940432,-94.9951224831991,
16.1016462681495));
#19894=CARTESIAN_POINT('Ctrl Pts',(-203.154555923984,-92.1268793206523,
16.2605545869538));
#19895=CARTESIAN_POINT('Ctrl Pts',(-206.415874511084,-91.8923173172992,
16.4194629057581));
#19896=CARTESIAN_POINT('Ctrl Pts',(-208.3789799615,-94.507596220001,16.5783712245624));
#19897=CARTESIAN_POINT('Ctrl Pts',(-207.24459588485,-97.5727507741492,16.7372795433667));
#19898=CARTESIAN_POINT('Ctrl Pts',(-204.051738814861,-98.2824665195066,
16.896187862171));
#19899=CARTESIAN_POINT('Ctrl Pts',(-201.729695881446,-95.9762200822744,
17.0550961809753));
#19900=CARTESIAN_POINT('Ctrl Pts',(-202.180151203454,-93.8537350466212,
17.1610350601782));
#19901=CARTESIAN_POINT('Ctrl Pts',(-202.804802895981,-93.1231365609213,
17.2140044997796));
#19902=CARTESIAN_POINT('Ctrl Pts',(-204.301933573839,-97.6111321859386,
-0.214004499779623));
#19903=CARTESIAN_POINT('Ctrl Pts',(-203.43290490324,-97.3788039485619,-0.161035060178188));
#19904=CARTESIAN_POINT('Ctrl Pts',(-201.960390513822,-95.9806854975158,
-0.0550961809753165));
#19905=CARTESIAN_POINT('Ctrl Pts',(-202.528669977177,-92.9711647174406,
0.10381213782899));
#19906=CARTESIAN_POINT('Ctrl Pts',(-205.367278707393,-91.8260000402438,
0.262720456633297));
#19907=CARTESIAN_POINT('Ctrl Pts',(-207.866954762541,-93.5885776702228,
0.421628775437603));
#19908=CARTESIAN_POINT('Ctrl Pts',(-207.739310807963,-96.6461600345297,
0.580537094241911));
#19909=CARTESIAN_POINT('Ctrl Pts',(-205.099778907598,-98.1940634759493,
0.739445413046217));
#19910=CARTESIAN_POINT('Ctrl Pts',(-202.369021569689,-96.8139259560427,
0.898353731850524));
#19911=CARTESIAN_POINT('Ctrl Pts',(-202.050194568866,-93.7706849533848,
1.05726205065483));
#19912=CARTESIAN_POINT('Ctrl Pts',(-204.435774879538,-91.8545225651544,
1.21617036945914));
#19913=CARTESIAN_POINT('Ctrl Pts',(-207.338602101016,-92.8220714922477,
1.37507868826344));
#19914=CARTESIAN_POINT('Ctrl Pts',(-208.097438777988,-95.786334108705,1.53398700706775));
#19915=CARTESIAN_POINT('Ctrl Pts',(-206.016571564894,-98.0296880301736,
1.69289532587206));
#19916=CARTESIAN_POINT('Ctrl Pts',(-203.003726113702,-97.4954609101786,
1.85180364467636));
#19917=CARTESIAN_POINT('Ctrl Pts',(-201.821040696633,-94.6734216280877,
2.01071196348067));
#19918=CARTESIAN_POINT('Ctrl Pts',(-203.552790389423,-92.1507864683822,
2.16962028228498));
#19919=CARTESIAN_POINT('Ctrl Pts',(-206.611325314735,-92.2402780806049,
2.32852860108928));
#19920=CARTESIAN_POINT('Ctrl Pts',(-208.192615376664,-94.8598520723894,
2.48743691989359));
#19921=CARTESIAN_POINT('Ctrl Pts',(-206.84695125948,-97.6079120362055,2.6463452386979));
#19922=CARTESIAN_POINT('Ctrl Pts',(-203.808022911705,-97.9650674327889,
2.8052535575022));
#19923=CARTESIAN_POINT('Ctrl Pts',(-201.861885816114,-95.6038821278479,
2.96416187630651));
#19924=CARTESIAN_POINT('Ctrl Pts',(-202.792736739874,-92.6890644467946,
3.12307019511082));
#19925=CARTESIAN_POINT('Ctrl Pts',(-205.747181945741,-91.8928866476054,
3.28197851391513));
#19926=CARTESIAN_POINT('Ctrl Pts',(-208.0166190971,-93.9452756444879,3.44088683271943));
#19927=CARTESIAN_POINT('Ctrl Pts',(-207.520453575278,-96.9646241410233,
3.59979515152374));
#19928=CARTESIAN_POINT('Ctrl Pts',(-204.713564386756,-98.1828271837715,
3.75870347032805));
#19929=CARTESIAN_POINT('Ctrl Pts',(-202.169276166769,-96.4830498379951,
3.91761178913235));
#19930=CARTESIAN_POINT('Ctrl Pts',(-202.220163918797,-93.4236289766044,
4.07652010793666));
#19931=CARTESIAN_POINT('Ctrl Pts',(-204.819574320358,-91.8094074506325,
4.23542842674097));
#19932=CARTESIAN_POINT('Ctrl Pts',(-207.584396968464,-93.1202855133552,
4.39433674554527));
#19933=CARTESIAN_POINT('Ctrl Pts',(-207.979873361138,-96.1544648082402,
4.55324506434958));
#19934=CARTESIAN_POINT('Ctrl Pts',(-205.643435161757,-98.1302436701516,
4.71215338315388));
#19935=CARTESIAN_POINT('Ctrl Pts',(-202.717102797615,-97.236250121351,4.8710617019582));
#19936=CARTESIAN_POINT('Ctrl Pts',(-201.883705073152,-94.2920874554028,
5.02997002076249));
#19937=CARTESIAN_POINT('Ctrl Pts',(-203.907291707438,-91.9969310981482,
5.18887833956681));
#19938=CARTESIAN_POINT('Ctrl Pts',(-206.932661091371,-92.4549547454316,
5.34778665837111));
#19939=CARTESIAN_POINT('Ctrl Pts',(-208.186188387689,-95.2462474366585,
5.50669497717542));
#19940=CARTESIAN_POINT('Ctrl Pts',(-206.518653781542,-97.8117832302136,
5.66560329597972));
#19941=CARTESIAN_POINT('Ctrl Pts',(-203.458834362157,-97.7995075850287,
5.82451161478403));
#19942=CARTESIAN_POINT('Ctrl Pts',(-201.811938374257,-95.220674675407,5.98341993358834));
#19943=CARTESIAN_POINT('Ctrl Pts',(-203.087821652533,-92.4395296898073,
6.14232825239265));
#19944=CARTESIAN_POINT('Ctrl Pts',(-206.116768667744,-92.0057952667451,
6.30123657119695));
#19945=CARTESIAN_POINT('Ctrl Pts',(-208.12187465026,-94.3171142775237,6.46014489000126));
#19946=CARTESIAN_POINT('Ctrl Pts',(-207.264880845966,-97.2544952861959,
6.61905320880556));
#19947=CARTESIAN_POINT('Ctrl Pts',(-204.331469596194,-98.1249802145116,
6.77796152760988));
#19948=CARTESIAN_POINT('Ctrl Pts',(-202.010959548606,-96.1305182094207,
6.93686984641417));
#19949=CARTESIAN_POINT('Ctrl Pts',(-202.430768378969,-93.0996097455012,
7.0957781652185));
#19950=CARTESIAN_POINT('Ctrl Pts',(-205.206020043722,-91.8109578266372,
7.25468648402278));
#19951=CARTESIAN_POINT('Ctrl Pts',(-207.792394835035,-93.4459841290473,
7.4135948028271));
#19952=CARTESIAN_POINT('Ctrl Pts',(-207.818733251607,-96.5057148130326,
7.5725031216314));
#19953=CARTESIAN_POINT('Ctrl Pts',(-205.260888527505,-98.1850229854928,
7.73141144043571));
#19954=CARTESIAN_POINT('Ctrl Pts',(-202.463864117283,-96.9443376831967,
7.89031975924002));
#19955=CARTESIAN_POINT('Ctrl Pts',(-201.99194073847,-93.921105324406,8.04922807804432));
#19956=CARTESIAN_POINT('Ctrl Pts',(-204.277772470171,-91.8869915456173,
8.20813639684863));
#19957=CARTESIAN_POINT('Ctrl Pts',(-207.225734329031,-92.7068491243547,
8.36704471565294));
#19958=CARTESIAN_POINT('Ctrl Pts',(-208.133167831608,-95.6290417958106,
8.52595303445724));
#19959=CARTESIAN_POINT('Ctrl Pts',(-206.168148084936,-97.9745359795373,
8.68486135326155));
#19960=CARTESIAN_POINT('Ctrl Pts',(-203.132183230144,-97.5930088229981,
8.84376967206586));
#19961=CARTESIAN_POINT('Ctrl Pts',(-201.808611913754,-94.8342401590575,
9.00267799087016));
#19962=CARTESIAN_POINT('Ctrl Pts',(-203.41086952535,-92.2274382646298,9.16158630967448));
#19963=CARTESIAN_POINT('Ctrl Pts',(-206.470024194722,-92.1624899808399,
9.32049462847878));
#19964=CARTESIAN_POINT('Ctrl Pts',(-208.18147711253,-94.6989391683534,9.47940294728308));
#19965=CARTESIAN_POINT('Ctrl Pts',(-206.976187372282,-97.5113975614257,
9.63831126608739));
#19966=CARTESIAN_POINT('Ctrl Pts',(-203.959151136564,-98.0214347395542,
9.7972195848917));
#19967=CARTESIAN_POINT('Ctrl Pts',(-201.896353505491,-95.7614543184109,
9.956127903696));
#19968=CARTESIAN_POINT('Ctrl Pts',(-202.678944291769,-92.8033810887658,
10.1150362225003));
#19969=CARTESIAN_POINT('Ctrl Pts',(-205.589453009393,-91.859143525785,10.2739445413046));
#19970=CARTESIAN_POINT('Ctrl Pts',(-207.9595577962,-93.7944080736608,10.4328528601089));
#19971=CARTESIAN_POINT('Ctrl Pts',(-207.616373073816,-96.8349458249529,
10.5917611789132));
#19972=CARTESIAN_POINT('Ctrl Pts',(-204.874526760019,-98.1932257527382,
10.7506694977175));
#19973=CARTESIAN_POINT('Ctrl Pts',(-202.247712910248,-96.6239920004371,
10.9095778165219));
#19974=CARTESIAN_POINT('Ctrl Pts',(-202.144165102618,-93.5659005331583,
11.0684861353261));
#19975=CARTESIAN_POINT('Ctrl Pts',(-204.658814809832,-91.8225754284465,
11.2273944541305));
#19976=CARTESIAN_POINT('Ctrl Pts',(-207.486259286036,-92.9922776575177,
11.3863027729348));
#19977=CARTESIAN_POINT('Ctrl Pts',(-208.034329037208,-96.0026372902789,
11.5452110917391));
#19978=CARTESIAN_POINT('Ctrl Pts',(-205.800559841136,-98.0937902615824,
11.7041194105434));
#19979=CARTESIAN_POINT('Ctrl Pts',(-202.832846330403,-97.3485908997207,
11.8630277293477));
#19980=CARTESIAN_POINT('Ctrl Pts',(-201.851955082127,-94.4502296507111,
12.021936048152));
#19981=CARTESIAN_POINT('Ctrl Pts',(-203.757156229511,-92.0558917132578,
12.1808443669563));
#19982=CARTESIAN_POINT('Ctrl Pts',(-206.80178265467,-92.3606793474046,12.3397526857606));
#19983=CARTESIAN_POINT('Ctrl Pts',(-208.194554880182,-95.0851666567005,
12.4986610045649));
#19984=CARTESIAN_POINT('Ctrl Pts',(-206.658594896419,-97.7315741270424,
12.6575693233692));
#19985=CARTESIAN_POINT('Ctrl Pts',(-203.602053649399,-97.8737049679119,
12.8164776421735));
#19986=CARTESIAN_POINT('Ctrl Pts',(-201.827133992036,-95.3812552130871,
12.9753859609778));
#19987=CARTESIAN_POINT('Ctrl Pts',(-202.961062428342,-92.5392749399473,
13.1342942797821));
#19988=CARTESIAN_POINT('Ctrl Pts',(-205.964266041489,-91.9532598991944,
13.2932025985864));
#19989=CARTESIAN_POINT('Ctrl Pts',(-208.083441325348,-94.1604621293612,
13.4521109173908));
#19990=CARTESIAN_POINT('Ctrl Pts',(-207.375752064809,-97.1373432974659,
13.6110192361951));
#19991=CARTESIAN_POINT('Ctrl Pts',(-204.489999865174,-98.1547320160434,
13.7699275549994));
#19992=CARTESIAN_POINT('Ctrl Pts',(-202.071810087677,-96.2798976884151,
13.9288358738037));
#19993=CARTESIAN_POINT('Ctrl Pts',(-202.33815209672,-93.231667452143,14.087744192608));
#19994=CARTESIAN_POINT('Ctrl Pts',(-205.044846506994,-91.8046247584532,
14.2466525114123));
#19995=CARTESIAN_POINT('Ctrl Pts',(-207.710426152417,-93.3070663163548,
14.4055608302166));
#19996=CARTESIAN_POINT('Ctrl Pts',(-207.891117371357,-96.3615706692395,
14.5644691490209));
#19997=CARTESIAN_POINT('Ctrl Pts',(-205.421264546907,-98.1678020119983,
14.7233774678252));
#19998=CARTESIAN_POINT('Ctrl Pts',(-202.565200992417,-97.0698283692467,
14.8822857866295));
#19999=CARTESIAN_POINT('Ctrl Pts',(-201.94133416535,-94.0742581918852,15.0411941054338));
#20000=CARTESIAN_POINT('Ctrl Pts',(-204.121617554176,-91.9273998656518,
15.2001024242381));
#20001=CARTESIAN_POINT('Ctrl Pts',(-207.107193051684,-92.5974626419489,
15.3590107430424));
#20002=CARTESIAN_POINT('Ctrl Pts',(-208.160915650643,-95.4701538272465,
15.5179190618468));
#20003=CARTESIAN_POINT('Ctrl Pts',(-206.316749956396,-97.9117946067699,
15.676827380651));
#20004=CARTESIAN_POINT('Ctrl Pts',(-203.265394666789,-97.6839731562328,
15.8357356994554));
#20005=CARTESIAN_POINT('Ctrl Pts',(-201.804322600784,-94.995435472909,15.9946440182597));
#20006=CARTESIAN_POINT('Ctrl Pts',(-203.272977864808,-92.3112471546551,
16.153552337064));
#20007=CARTESIAN_POINT('Ctrl Pts',(-206.325018001399,-92.091736968933,16.3124606558683));
#20008=CARTESIAN_POINT('Ctrl Pts',(-208.162151193701,-94.5391937157227,
16.4713689746726));
#20009=CARTESIAN_POINT('Ctrl Pts',(-207.100560416909,-97.4076576435095,
16.6302772934769));
#20010=CARTESIAN_POINT('Ctrl Pts',(-204.112588629499,-98.0718310085313,
16.7891856122812));
#20011=CARTESIAN_POINT('Ctrl Pts',(-201.939550932507,-95.9135761483203,
16.9480939310855));
#20012=CARTESIAN_POINT('Ctrl Pts',(-202.36110058667,-93.9272907410154,17.0540328102884));
#20013=CARTESIAN_POINT('Ctrl Pts',(-202.945668449658,-93.2435746787732,
17.1070022498898));
#20014=CARTESIAN_POINT('Ctrl Pts',(-204.349800002025,-97.4320868020351,
-0.321006749669434));
#20015=CARTESIAN_POINT('Ctrl Pts',(-203.540360643981,-97.2156893163364,
-0.268037310067998));
#20016=CARTESIAN_POINT('Ctrl Pts',(-202.168816594393,-95.9134398742047,
-0.162098430865127));
#20017=CARTESIAN_POINT('Ctrl Pts',(-202.698129124083,-93.1102819915483,
-0.00319011206082018));
#20018=CARTESIAN_POINT('Ctrl Pts',(-205.342094399406,-92.0436412781577,
0.155718206743486));
#20019=CARTESIAN_POINT('Ctrl Pts',(-207.67036761967,-93.685358926356,0.314626525547793));
#20020=CARTESIAN_POINT('Ctrl Pts',(-207.551476213497,-96.5332828094945,
0.4735348443521));
#20021=CARTESIAN_POINT('Ctrl Pts',(-205.092937065996,-97.9750464823464,
0.632443163156407));
#20022=CARTESIAN_POINT('Ctrl Pts',(-202.549427810949,-96.6895450185623,
0.791351481960713));
#20023=CARTESIAN_POINT('Ctrl Pts',(-202.252462783667,-93.8549791096304,
0.95025980076502));
#20024=CARTESIAN_POINT('Ctrl Pts',(-204.474463806834,-92.0702080129899,
1.10916811956933));
#20025=CARTESIAN_POINT('Ctrl Pts',(-207.178244110245,-92.971412091657,1.26807643837363));
#20026=CARTESIAN_POINT('Ctrl Pts',(-207.885047341772,-95.7324151638398,
1.42698475717794));
#20027=CARTESIAN_POINT('Ctrl Pts',(-205.946865233257,-97.8219422640298,
1.58589307598225));
#20028=CARTESIAN_POINT('Ctrl Pts',(-203.140610652246,-97.3243471078651,
1.74480139478655));
#20029=CARTESIAN_POINT('Ctrl Pts',(-202.039021996833,-94.6958151132924,
1.90370971359086));
#20030=CARTESIAN_POINT('Ctrl Pts',(-203.652025580085,-92.3461570947101,
2.06261803239517));
#20031=CARTESIAN_POINT('Ctrl Pts',(-206.500836707101,-92.4295122653719,
2.22152635119947));
#20032=CARTESIAN_POINT('Ctrl Pts',(-207.973697679257,-94.8694620184648,
2.38043467000378));
#20033=CARTESIAN_POINT('Ctrl Pts',(-206.720305776311,-97.4290874580306,
2.53934298880809));
#20034=CARTESIAN_POINT('Ctrl Pts',(-203.889756803435,-97.7617527022432,
2.69825130761239));
#20035=CARTESIAN_POINT('Ctrl Pts',(-202.07706636569,-95.5624739187976,2.8571596264167));
#20036=CARTESIAN_POINT('Ctrl Pts',(-202.944088823814,-92.8475253418532,
3.01606794522101));
#20037=CARTESIAN_POINT('Ctrl Pts',(-205.695947665438,-92.1059414695739,
3.17497626402532));
#20038=CARTESIAN_POINT('Ctrl Pts',(-207.809769467947,-94.0175981137072,
3.33388458282962));
#20039=CARTESIAN_POINT('Ctrl Pts',(-207.347626025441,-96.829909826118,3.49279290163393));
#20040=CARTESIAN_POINT('Ctrl Pts',(-204.733205282231,-97.9645806629382,
3.65170122043823));
#20041=CARTESIAN_POINT('Ctrl Pts',(-202.363378954125,-96.3813570822541,
3.81060953924254));
#20042=CARTESIAN_POINT('Ctrl Pts',(-202.410777332023,-93.5317207678121,
3.96951785804685));
#20043=CARTESIAN_POINT('Ctrl Pts',(-204.831946112661,-92.0281864427333,
4.12842617685115));
#20044=CARTESIAN_POINT('Ctrl Pts',(-207.407184818934,-93.2491775716366,
4.28733449565546));
#20045=CARTESIAN_POINT('Ctrl Pts',(-207.775543387802,-96.0753031342707,
4.44624281445976));
#20046=CARTESIAN_POINT('Ctrl Pts',(-205.599314800415,-97.9156028018523,
4.60515113326408));
#20047=CARTESIAN_POINT('Ctrl Pts',(-202.873641102421,-97.0829104077825,
4.76405945206838));
#20048=CARTESIAN_POINT('Ctrl Pts',(-202.097389475856,-94.340629032118,4.92296777087269));
#20049=CARTESIAN_POINT('Ctrl Pts',(-203.982218735947,-92.2028515901542,
5.08187608967699));
#20050=CARTESIAN_POINT('Ctrl Pts',(-206.800138483392,-92.6294685471878,
5.2407844084813));
#20051=CARTESIAN_POINT('Ctrl Pts',(-207.967711389038,-95.2293622452196,
5.39969272728561));
#20052=CARTESIAN_POINT('Ctrl Pts',(-206.414519662711,-97.6189792003685,
5.55860104608991));
#20053=CARTESIAN_POINT('Ctrl Pts',(-203.564512119404,-97.6075452964086,
5.71750936489422));
#20054=CARTESIAN_POINT('Ctrl Pts',(-202.030543820876,-95.2055430086959,
5.87641768369853));
#20055=CARTESIAN_POINT('Ctrl Pts',(-203.218939758371,-92.6151011879226,
6.03532600250283));
#20056=CARTESIAN_POINT('Ctrl Pts',(-206.040191818849,-92.2111079425408,
6.19423432130715));
#20057=CARTESIAN_POINT('Ctrl Pts',(-207.907807645815,-94.3639397645677,
6.35314264011144));
#20058=CARTESIAN_POINT('Ctrl Pts',(-207.109577923063,-97.0999045013251,
6.51205095891576));
#20059=CARTESIAN_POINT('Ctrl Pts',(-204.377310738763,-97.9107002614662,
6.67095927772006));
#20060=CARTESIAN_POINT('Ctrl Pts',(-202.215918109496,-96.05299855419,6.82986759652437));
#20061=CARTESIAN_POINT('Ctrl Pts',(-202.606940640336,-93.2299195415795,
6.98877591532867));
#20062=CARTESIAN_POINT('Ctrl Pts',(-205.191893245386,-92.0296305094257,
7.14768423413299));
#20063=CARTESIAN_POINT('Ctrl Pts',(-207.600920267818,-93.5525430270246,
7.30659255293729));
#20064=CARTESIAN_POINT('Ctrl Pts',(-207.625452658662,-96.4024679195202,
7.4655008717416));
#20065=CARTESIAN_POINT('Ctrl Pts',(-205.242999396187,-97.9666258984934,
7.6244091905459));
#20066=CARTESIAN_POINT('Ctrl Pts',(-202.637767003241,-96.8110144110925,
7.78331750935021));
#20067=CARTESIAN_POINT('Ctrl Pts',(-202.198203419534,-93.9950851529353,
7.94222582815451));
#20068=CARTESIAN_POINT('Ctrl Pts',(-204.327295625697,-92.1004505948418,
8.10113414695882));
#20069=CARTESIAN_POINT('Ctrl Pts',(-207.073115683543,-92.8640905237329,
8.26004246576312));
#20070=CARTESIAN_POINT('Ctrl Pts',(-207.918326453502,-95.5859083878473,
8.41895078456744));
#20071=CARTESIAN_POINT('Ctrl Pts',(-206.088048148422,-97.7705719905599,
8.57785910337173));
#20072=CARTESIAN_POINT('Ctrl Pts',(-203.260259461758,-97.4152061584378,
8.73676742217605));
#20073=CARTESIAN_POINT('Ctrl Pts',(-202.027445455834,-94.8456063145195,
8.89567574098035));
#20074=CARTESIAN_POINT('Ctrl Pts',(-203.519836232374,-92.4175528758237,
9.05458405978466));
#20075=CARTESIAN_POINT('Ctrl Pts',(-206.369224607589,-92.3570580970949,
9.21349237858896));
#20076=CARTESIAN_POINT('Ctrl Pts',(-207.963323166107,-94.7195829153344,
9.37240069739328));
#20077=CARTESIAN_POINT('Ctrl Pts',(-206.840680166388,-97.3391909826315,
9.53130901619757));
#20078=CARTESIAN_POINT('Ctrl Pts',(-204.030522163026,-97.814254901706,9.6902173350019));
#20079=CARTESIAN_POINT('Ctrl Pts',(-202.109170604948,-95.7092413812417,
9.84912565380619));
#20080=CARTESIAN_POINT('Ctrl Pts',(-202.838099126052,-92.9540032894992,
10.0080339726105));
#20081=CARTESIAN_POINT('Ctrl Pts',(-205.549034205271,-92.0745121142617,
10.1669422914148));
#20082=CARTESIAN_POINT('Ctrl Pts',(-207.75662086154,-93.8770755350957,10.3258506102191));
#20083=CARTESIAN_POINT('Ctrl Pts',(-207.436968322131,-96.7091235546594,
10.4847589290234));
#20084=CARTESIAN_POINT('Ctrl Pts',(-204.883130462482,-97.974266201832,10.6436672478277));
#20085=CARTESIAN_POINT('Ctrl Pts',(-202.436437288604,-96.5126348379233,
10.802575566632));
#20086=CARTESIAN_POINT('Ctrl Pts',(-202.339989756123,-93.6642367610134,
10.9614838854363));
#20087=CARTESIAN_POINT('Ctrl Pts',(-204.682209884844,-92.0404514920568,
11.1203922042406));
#20088=CARTESIAN_POINT('Ctrl Pts',(-207.315776439265,-93.1299472169208,
11.279300523045));
#20089=CARTESIAN_POINT('Ctrl Pts',(-207.826265037123,-95.9338864321184,
11.4382088418493));
#20090=CARTESIAN_POINT('Ctrl Pts',(-205.745665437526,-97.8816490042056,
11.5971171606536));
#20091=CARTESIAN_POINT('Ctrl Pts',(-202.981448098954,-97.1875479768318,
11.7560254794579));
#20092=CARTESIAN_POINT('Ctrl Pts',(-202.067816582323,-94.4879274140711,
11.9149337982622));
#20093=CARTESIAN_POINT('Ctrl Pts',(-203.842378050611,-92.2577692747585,
12.0738421170665));
#20094=CARTESIAN_POINT('Ctrl Pts',(-206.678234383597,-92.5416576150057,
12.2327504358708));
#20095=CARTESIAN_POINT('Ctrl Pts',(-207.975504190982,-95.0793267774225,
12.3916587546751));
#20096=CARTESIAN_POINT('Ctrl Pts',(-206.544865012666,-97.544270036935,12.5505670734794));
#20097=CARTESIAN_POINT('Ctrl Pts',(-203.697910857383,-97.6766549633293,
12.7094753922837));
#20098=CARTESIAN_POINT('Ctrl Pts',(-202.044697474854,-95.3551125358376,
12.868383711088));
#20099=CARTESIAN_POINT('Ctrl Pts',(-203.100872416607,-92.7080069043539,
13.0272920298923));
#20100=CARTESIAN_POINT('Ctrl Pts',(-205.898146300591,-92.1621749261473,
13.1862003486966));
#20101=CARTESIAN_POINT('Ctrl Pts',(-207.872009694727,-94.2180292571993,
13.3451086675009));
#20102=CARTESIAN_POINT('Ctrl Pts',(-207.212846700311,-96.9907856267017,
13.5040169863053));
#20103=CARTESIAN_POINT('Ctrl Pts',(-204.524970584168,-97.9384119813983,
13.6629253051096));
#20104=CARTESIAN_POINT('Ctrl Pts',(-202.272596125939,-96.1921350794542,
13.8218336239139));
#20105=CARTESIAN_POINT('Ctrl Pts',(-202.520675058331,-93.3529220487526,
13.9807419427182));
#20106=CARTESIAN_POINT('Ctrl Pts',(-205.041771381152,-92.0237316998481,
14.1396502615225));
#20107=CARTESIAN_POINT('Ctrl Pts',(-207.524572179335,-93.423150811404,14.2985585803268));
#20108=CARTESIAN_POINT('Ctrl Pts',(-207.692873397937,-96.2682077424223,
14.4574668991311));
#20109=CARTESIAN_POINT('Ctrl Pts',(-205.392378428873,-97.9505857674807,
14.6163752179354));
#20110=CARTESIAN_POINT('Ctrl Pts',(-202.73215520691,-96.9279001984011,14.7752835367397));
#20111=CARTESIAN_POINT('Ctrl Pts',(-202.151066940101,-94.1377363253639,
14.934191855544));
#20112=CARTESIAN_POINT('Ctrl Pts',(-204.181848255277,-92.1380881155991,
15.0931001743483));
#20113=CARTESIAN_POINT('Ctrl Pts',(-206.962702783849,-92.7622046745167,
15.2520084931526));
#20114=CARTESIAN_POINT('Ctrl Pts',(-207.944171604055,-95.4379153703248,
15.4109168119569));
#20115=CARTESIAN_POINT('Ctrl Pts',(-206.226460386715,-97.7121327949226,
15.5698251307612));
#20116=CARTESIAN_POINT('Ctrl Pts',(-203.384336587646,-97.4999330656037,
15.7287334495655));
#20117=CARTESIAN_POINT('Ctrl Pts',(-202.023450261136,-94.9957484626189,
15.8876417683698));
#20118=CARTESIAN_POINT('Ctrl Pts',(-203.391399805631,-92.4956149886579,
16.0465500871742));
#20119=CARTESIAN_POINT('Ctrl Pts',(-206.234161491715,-92.2911566205669,
16.2054584059785));
#20120=CARTESIAN_POINT('Ctrl Pts',(-207.945322425902,-94.5707912114442,
16.3643667247828));
#20121=CARTESIAN_POINT('Ctrl Pts',(-206.956524948968,-97.24256451287,16.5232750435871));
#20122=CARTESIAN_POINT('Ctrl Pts',(-204.173438444138,-97.8611954975559,
16.6821833623914));
#20123=CARTESIAN_POINT('Ctrl Pts',(-202.149405983567,-95.8509322143663,
16.8410916811957));
#20124=CARTESIAN_POINT('Ctrl Pts',(-202.542049969887,-94.0008464354096,
16.9470305603986));
#20125=CARTESIAN_POINT('Ctrl Pts',(-203.086534003335,-93.3640127966251,
17.));
#20126=CARTESIAN_POINT('Ctrl Pts',(-202.485813979692,-94.9986458132734,
0.887416697508031));
#20127=CARTESIAN_POINT('Ctrl Pts',(-202.484186104837,-94.6662414532709,
0.908364398593701));
#20128=CARTESIAN_POINT('Ctrl Pts',(-202.545408874051,-94.3344113220432,
0.92931209967937));
#20129=CARTESIAN_POINT('Ctrl Pts',(-202.672290458742,-94.029944911679,0.95025980076504));
#20130=CARTESIAN_POINT('Ctrl Pts',(-202.993129791389,-93.2600554107502,
1.00322924036648));
#20131=CARTESIAN_POINT('Ctrl Pts',(-203.733796799112,-92.6651317118701,
1.05619867996791));
#20132=CARTESIAN_POINT('Ctrl Pts',(-204.554760353541,-92.5178705422078,
1.10916811956935));
#20133=CARTESIAN_POINT('Ctrl Pts',(-205.375723907971,-92.3706093725456,
1.16213755917078));
#20134=CARTESIAN_POINT('Ctrl Pts',(-206.276984009108,-92.6710107321013,
1.21510699877222));
#20135=CARTESIAN_POINT('Ctrl Pts',(-206.845414598264,-93.2813785905763,
1.26807643837365));
#20136=CARTESIAN_POINT('Ctrl Pts',(-207.41384518742,-93.8917464490512,1.32104587797509));
#20137=CARTESIAN_POINT('Ctrl Pts',(-207.649446264596,-94.8120808064455,
1.37401531757652));
#20138=CARTESIAN_POINT('Ctrl Pts',(-207.444216451765,-95.620502501841,1.42698475717796));
#20139=CARTESIAN_POINT('Ctrl Pts',(-207.238986638933,-96.4289241972365,
1.4799541967794));
#20140=CARTESIAN_POINT('Ctrl Pts',(-206.592925936095,-97.1254332306331,
1.53292363638083));
#20141=CARTESIAN_POINT('Ctrl Pts',(-205.802186487841,-97.390755221304,1.58589307598227));
#20142=CARTESIAN_POINT('Ctrl Pts',(-205.011447039586,-97.6560772119749,
1.6388625155837));
#20143=CARTESIAN_POINT('Ctrl Pts',(-204.076028845916,-97.49021215992,1.69183195518514));
#20144=CARTESIAN_POINT('Ctrl Pts',(-203.424721639845,-96.9691909681305,
1.74480139478657));
#20145=CARTESIAN_POINT('Ctrl Pts',(-202.840193560653,-96.501590558344,1.79233982902706));
#20146=CARTESIAN_POINT('Ctrl Pts',(-202.484502889507,-95.7479293694392,
1.83987826326755));
#20147=CARTESIAN_POINT('Ctrl Pts',(-202.479323384637,-94.9985362448309,
1.88741669750803));
#20148=CARTESIAN_POINT('Ctrl Pts',(-204.206200717467,-97.9692229537457,
-1.94289029309402E-15));
#20149=CARTESIAN_POINT('Ctrl Pts',(-204.113164566746,-97.9351899142219,
-1.95608846886529E-15));
#20150=CARTESIAN_POINT('Ctrl Pts',(-204.022195793433,-97.8963847243652,
-1.87178471689281E-15));
#20151=CARTESIAN_POINT('Ctrl Pts',(-203.933501803929,-97.8531368677882,
-1.96197225132977E-15));
#20152=CARTESIAN_POINT('Ctrl Pts',(-203.842828758516,-97.808924008661,-2.05417216759616E-15));
#20153=CARTESIAN_POINT('Ctrl Pts',(-203.754532478722,-97.7600673920919,
-2.02940294614423E-15));
#20154=CARTESIAN_POINT('Ctrl Pts',(-203.668863497467,-97.706873479352,-1.98105420956551E-15));
#20155=CARTESIAN_POINT('Ctrl Pts',(-203.585835066753,-97.6553191473921,
-1.93419571228578E-15));
#20156=CARTESIAN_POINT('Ctrl Pts',(-203.505274137607,-97.5996899115334,
-2.24355396026084E-15));
#20157=CARTESIAN_POINT('Ctrl Pts',(-203.427442606602,-97.5402339590788,
-2.26207941267376E-15));
#20158=CARTESIAN_POINT('Ctrl Pts',(-203.359340016973,-97.4882100006811,
-2.27828918353506E-15));
#20159=CARTESIAN_POINT('Ctrl Pts',(-203.29332742065,-97.4332554915952,-1.79029168246463E-15));
#20160=CARTESIAN_POINT('Ctrl Pts',(-203.2296056295,-97.3755236839992,-1.74166236988071E-15));
#20161=CARTESIAN_POINT('Ctrl Pts',(-203.216356113094,-97.3635196502445,
-1.73155099568283E-15));
#20162=CARTESIAN_POINT('Ctrl Pts',(-203.203203983489,-97.3513937509761,
-1.77457247924768E-15));
#20163=CARTESIAN_POINT('Ctrl Pts',(-203.190167931591,-97.3391634026804,
-1.77635683940025E-15));
#20164=CARTESIAN_POINT('Ctrl Pts',(-203.117744760303,-97.2712164033532,
-1.78627004180089E-15));
#20165=CARTESIAN_POINT('Ctrl Pts',(-203.048787400483,-97.1999474448534,
-1.60673788718679E-15));
#20166=CARTESIAN_POINT('Ctrl Pts',(-202.983534963279,-97.1256486442048,
-1.63757896132211E-15));
#20167=CARTESIAN_POINT('Ctrl Pts',(-202.918640645489,-97.0517576113602,
-1.66825077300687E-15));
#20168=CARTESIAN_POINT('Ctrl Pts',(-202.857410209928,-96.97486910218,-1.76356714015849E-15));
#20169=CARTESIAN_POINT('Ctrl Pts',(-202.800122474302,-96.8952437100093,
-1.72084568816899E-15));
#20170=CARTESIAN_POINT('Ctrl Pts',(-202.744171289059,-96.8174760164764,
-1.67912094817054E-15));
#20171=CARTESIAN_POINT('Ctrl Pts',(-202.691980694321,-96.7370969139694,
-2.11654729638491E-15));
#20172=CARTESIAN_POINT('Ctrl Pts',(-202.643857601275,-96.6543350073822,
-2.27595720048157E-15));
#20173=CARTESIAN_POINT('Ctrl Pts',(-202.62307823217,-96.6185987299325,-2.34478979262376E-15));
#20174=CARTESIAN_POINT('Ctrl Pts',(-202.603057870683,-96.5824180660604,
-2.21214957918682E-15));
#20175=CARTESIAN_POINT('Ctrl Pts',(-202.583824240712,-96.5458110879139,
-2.23432383705813E-15));
#20176=CARTESIAN_POINT('Ctrl Pts',(-202.569909304535,-96.5193270718798,
-2.25036622653533E-15));
#20177=CARTESIAN_POINT('Ctrl Pts',(-202.55640618783,-96.4926199163307,-1.6439290738235E-15));
#20178=CARTESIAN_POINT('Ctrl Pts',(-202.543326026024,-96.4656964618893,
-1.63757896132211E-15));
#20179=CARTESIAN_POINT('Ctrl Pts',(-202.537164434797,-96.4530137960989,
-1.63458765295335E-15));
#20180=CARTESIAN_POINT('Ctrl Pts',(-202.531098886162,-96.4402875329931,
-2.24077876564333E-15));
#20181=CARTESIAN_POINT('Ctrl Pts',(-202.525133543247,-96.4275255114806,
-2.23432383705813E-15));
#20182=CARTESIAN_POINT('Ctrl Pts',(-202.485117270381,-96.3419162611141,
-2.19102336175286E-15));
#20183=CARTESIAN_POINT('Ctrl Pts',(-202.4495592445,-96.254603019968,-1.8759278374734E-15));
#20184=CARTESIAN_POINT('Ctrl Pts',(-202.418711175416,-96.1658234873367,
-1.80411241501588E-15));
#20185=CARTESIAN_POINT('Ctrl Pts',(-202.388547336981,-96.0790131436709,
-1.73388990629946E-15));
#20186=CARTESIAN_POINT('Ctrl Pts',(-202.362886617194,-95.990800160075,-1.72432441326592E-15));
#20187=CARTESIAN_POINT('Ctrl Pts',(-202.342013530391,-95.9013982186672,
-1.63757896132211E-15));
#20188=CARTESIAN_POINT('Ctrl Pts',(-202.338634312827,-95.886924623388,-1.62353543448175E-15));
#20189=CARTESIAN_POINT('Ctrl Pts',(-202.335380687559,-95.8724198597991,
-2.0203055504241E-15));
#20190=CARTESIAN_POINT('Ctrl Pts',(-202.332253992484,-95.8578848308905,
-2.02615701994091E-15));
#20191=CARTESIAN_POINT('Ctrl Pts',(-202.312215595091,-95.7647325795669,
-2.03483094975162E-15));
#20192=CARTESIAN_POINT('Ctrl Pts',(-202.297386480098,-95.670336192193,-1.24180755483495E-15));
#20193=CARTESIAN_POINT('Ctrl Pts',(-202.287688067001,-95.5751039661889,
-1.16573417585641E-15));
#20194=CARTESIAN_POINT('Ctrl Pts',(-202.284332121912,-95.5421507275438,
-1.13941047938093E-15));
#20195=CARTESIAN_POINT('Ctrl Pts',(-202.281590951551,-95.5090975364209,
-1.59096596101214E-15));
#20196=CARTESIAN_POINT('Ctrl Pts',(-202.27946265438,-95.4759618339203,-1.58206781009085E-15));
#20197=CARTESIAN_POINT('Ctrl Pts',(-202.278435478218,-95.459969610567,-1.57777331182387E-15));
#20198=CARTESIAN_POINT('Ctrl Pts',(-202.277551068544,-95.4439581729582,
-1.39634750300735E-15));
#20199=CARTESIAN_POINT('Ctrl Pts',(-202.276809266428,-95.4279295130754,
-1.36002320516582E-15));
#20200=CARTESIAN_POINT('Ctrl Pts',(-202.276232614801,-95.4154693803712,
-1.33178593674769E-15));
#20201=CARTESIAN_POINT('Ctrl Pts',(-202.27574223997,-95.402999988249,-2.11721333807556E-15));
#20202=CARTESIAN_POINT('Ctrl Pts',(-202.275338217547,-95.3905321636395,
-2.1094237467878E-15));
#20203=CARTESIAN_POINT('Ctrl Pts',(-202.272318895462,-95.2973581810847,
-2.05121092574771E-15));
#20204=CARTESIAN_POINT('Ctrl Pts',(-202.274110299127,-95.2041209575845,
-1.64901362259784E-15));
#20205=CARTESIAN_POINT('Ctrl Pts',(-202.280572742583,-95.111194847899,-1.63757896132211E-15));
#20206=CARTESIAN_POINT('Ctrl Pts',(-202.287048682582,-95.0180746659159,
-1.62612041923403E-15));
#20207=CARTESIAN_POINT('Ctrl Pts',(-202.29821557696,-94.9252659180417,-1.50579107067496E-15));
#20208=CARTESIAN_POINT('Ctrl Pts',(-202.313983936443,-94.8331572852858,
-1.4432899320127E-15));
#20209=CARTESIAN_POINT('Ctrl Pts',(-202.329531074206,-94.7423408877986,
-1.38166565117914E-15));
#20210=CARTESIAN_POINT('Ctrl Pts',(-202.349551938789,-94.6522042518842,
-1.95220788294063E-15));
#20211=CARTESIAN_POINT('Ctrl Pts',(-202.374003831615,-94.5631450482855,
-2.02615701994091E-15));
#20212=CARTESIAN_POINT('Ctrl Pts',(-202.383516776035,-94.5284967999894,
-2.0549267366747E-15));
#20213=CARTESIAN_POINT('Ctrl Pts',(-202.393700820255,-94.4940119683205,
-2.105212970477E-15));
#20214=CARTESIAN_POINT('Ctrl Pts',(-202.40455502065,-94.4597154343389,-2.13717932240343E-15));
#20215=CARTESIAN_POINT('Ctrl Pts',(-202.410353854707,-94.4413925821662,
-2.15425727964432E-15));
#20216=CARTESIAN_POINT('Ctrl Pts',(-202.416343979603,-94.4231234896604,
-1.92388717056435E-15));
#20217=CARTESIAN_POINT('Ctrl Pts',(-202.422525347087,-94.4049120649473,
-1.9151347174784E-15));
#20218=CARTESIAN_POINT('Ctrl Pts',(-202.428042996055,-94.3886560748213,
-1.90732205080426E-15));
#20219=CARTESIAN_POINT('Ctrl Pts',(-202.433713565198,-94.3724447894493,
-2.11171038093633E-15));
#20220=CARTESIAN_POINT('Ctrl Pts',(-202.43953069679,-94.3562979493254,-2.1094237467878E-15));
#20221=CARTESIAN_POINT('Ctrl Pts',(-202.470363841107,-94.2707131823399,
-2.09730366327417E-15));
#20222=CARTESIAN_POINT('Ctrl Pts',(-202.505347374394,-94.1868267447458,
-2.98179513899234E-15));
#20223=CARTESIAN_POINT('Ctrl Pts',(-202.544417035463,-94.1050192581487,
-2.4980018054066E-15));
#20224=CARTESIAN_POINT('Ctrl Pts',(-202.5758795135,-94.0391403592833,-2.10840699665774E-15));
#20225=CARTESIAN_POINT('Ctrl Pts',(-202.609992739017,-93.9746099539844,
-1.67224799697884E-15));
#20226=CARTESIAN_POINT('Ctrl Pts',(-202.646741355094,-93.9116445196917,
-1.77635683940025E-15));
#20227=CARTESIAN_POINT('Ctrl Pts',(-202.661983680304,-93.8855281722226,
-1.81953835214335E-15));
#20228=CARTESIAN_POINT('Ctrl Pts',(-202.677679568848,-93.8596812729456,
-2.49009010979644E-15));
#20229=CARTESIAN_POINT('Ctrl Pts',(-202.693828658099,-93.8341202619796,
-2.55351295663786E-15));
#20230=CARTESIAN_POINT('Ctrl Pts',(-202.702295534382,-93.8207187683019,
-2.58676519701672E-15));
#20231=CARTESIAN_POINT('Ctrl Pts',(-202.710885570826,-93.8073982241056,
-2.09795412669662E-15));
#20232=CARTESIAN_POINT('Ctrl Pts',(-202.719593908756,-93.7941678734082,
-2.05391259555654E-15));
#20233=CARTESIAN_POINT('Ctrl Pts',(-202.767002638161,-93.7221410272768,
-1.81414778059626E-15));
#20234=CARTESIAN_POINT('Ctrl Pts',(-202.817953827573,-93.6527223685765,
-9.92560611046316E-16));
#20235=CARTESIAN_POINT('Ctrl Pts',(-202.872410768078,-93.5862671725324,
-6.66133814775094E-16));
#20236=CARTESIAN_POINT('Ctrl Pts',(-202.926867708583,-93.5198119764882,
-3.3970701850387E-16));
#20237=CARTESIAN_POINT('Ctrl Pts',(-202.984830731065,-93.4563195512772,
-4.53570776702435E-17));
#20238=CARTESIAN_POINT('Ctrl Pts',(-203.046292621091,-93.3961891673829,
3.33066907387547E-16));
#20239=CARTESIAN_POINT('Ctrl Pts',(-203.058343397196,-93.3843994584574,
4.07452946255978E-16));
#20240=CARTESIAN_POINT('Ctrl Pts',(-203.070528764207,-93.3727391521122,
-1.78805262136535E-16));
#20241=CARTESIAN_POINT('Ctrl Pts',(-203.082846138209,-93.3612093103597,
-1.66533453693773E-16));
#20242=CARTESIAN_POINT('Origin',(-205.,-95.,9.));
#20243=CARTESIAN_POINT('Origin',(-205.,95.,17.));
#20244=CARTESIAN_POINT('Ctrl Pts',(-203.086534003335,96.6359872033749,17.));
#20245=CARTESIAN_POINT('Ctrl Pts',(-203.024407982535,96.5776039990143,17.));
#20246=CARTESIAN_POINT('Ctrl Pts',(-202.965660663619,96.5159659235685,17.));
#20247=CARTESIAN_POINT('Ctrl Pts',(-202.910302607292,96.4514497134767,17.));
#20248=CARTESIAN_POINT('Ctrl Pts',(-202.853587227097,96.3853516307974,17.));
#20249=CARTESIAN_POINT('Ctrl Pts',(-202.800428883688,96.3162320542646,17.));
#20250=CARTESIAN_POINT('Ctrl Pts',(-202.750867872641,96.2444498370416,17.));
#20251=CARTESIAN_POINT('Ctrl Pts',(-202.73795912874,96.2257533205829,17.));
#20252=CARTESIAN_POINT('Ctrl Pts',(-202.725294599279,96.2068759539151,17.));
#20253=CARTESIAN_POINT('Ctrl Pts',(-202.712875369652,96.1878236473054,17.));
#20254=CARTESIAN_POINT('Ctrl Pts',(-202.702666789577,96.1721626921996,17.));
#20255=CARTESIAN_POINT('Ctrl Pts',(-202.692623482104,96.1563825746979,17.));
#20256=CARTESIAN_POINT('Ctrl Pts',(-202.682754989924,96.1405013265158,17.));
#20257=CARTESIAN_POINT('Ctrl Pts',(-202.635325886293,96.0641742289145,17.));
#20258=CARTESIAN_POINT('Ctrl Pts',(-202.591881571366,95.9854386369538,17.));
#20259=CARTESIAN_POINT('Ctrl Pts',(-202.55245519555,95.9046876041234,17.));
#20260=CARTESIAN_POINT('Ctrl Pts',(-202.520329458461,95.8388893562068,17.));
#20261=CARTESIAN_POINT('Ctrl Pts',(-202.490871898904,95.7717518764231,17.));
#20262=CARTESIAN_POINT('Ctrl Pts',(-202.464118215874,95.7034693999465,17.));
#20263=CARTESIAN_POINT('Ctrl Pts',(-202.455239378807,95.6808082589538,17.));
#20264=CARTESIAN_POINT('Ctrl Pts',(-202.446658487047,95.6580208940291,17.));
#20265=CARTESIAN_POINT('Ctrl Pts',(-202.438377277411,95.6351140931728,17.));
#20266=CARTESIAN_POINT('Ctrl Pts',(-202.431690505786,95.6166176955754,17.));
#20267=CARTESIAN_POINT('Ctrl Pts',(-202.425198327662,95.5980406868312,17.));
#20268=CARTESIAN_POINT('Ctrl Pts',(-202.418909348376,95.5794101202441,17.));
#20269=CARTESIAN_POINT('Ctrl Pts',(-202.389394173141,95.4919739223399,17.));
#20270=CARTESIAN_POINT('Ctrl Pts',(-202.364312526072,95.4032571051593,17.));
#20271=CARTESIAN_POINT('Ctrl Pts',(-202.343695486232,95.3136579957359,17.));
#20272=CARTESIAN_POINT('Ctrl Pts',(-202.322619877632,95.2220660031035,17.));
#20273=CARTESIAN_POINT('Ctrl Pts',(-202.306209135304,95.1295512442093,17.));
#20274=CARTESIAN_POINT('Ctrl Pts',(-202.294539294593,95.0365052928358,17.));
#20275=CARTESIAN_POINT('Ctrl Pts',(-202.28303676288,94.9447933292428,17.));
#20276=CARTESIAN_POINT('Ctrl Pts',(-202.276139875649,94.8525643337987,17.));
#20277=CARTESIAN_POINT('Ctrl Pts',(-202.273968539135,94.7601740929499,17.));
#20278=CARTESIAN_POINT('Ctrl Pts',(-202.272844064581,94.712327766861,17.));
#20279=CARTESIAN_POINT('Ctrl Pts',(-202.272987744046,94.6644379678861,17.));
#20280=CARTESIAN_POINT('Ctrl Pts',(-202.274421710976,94.6165533352961,17.));
#20281=CARTESIAN_POINT('Ctrl Pts',(-202.275071818331,94.5948442211265,17.));
#20282=CARTESIAN_POINT('Ctrl Pts',(-202.27598770662,94.5731290901658,17.));
#20283=CARTESIAN_POINT('Ctrl Pts',(-202.277169213423,94.5514506162179,17.));
#20284=CARTESIAN_POINT('Ctrl Pts',(-202.282380583036,94.4558315812025,17.));
#20285=CARTESIAN_POINT('Ctrl Pts',(-202.292755622429,94.3608204174972,17.));
#20286=CARTESIAN_POINT('Ctrl Pts',(-202.308361288381,94.2668143079404,17.));
#20287=CARTESIAN_POINT('Ctrl Pts',(-202.312210020092,94.2436301454694,17.));
#20288=CARTESIAN_POINT('Ctrl Pts',(-202.316377126191,94.2205070204909,17.));
#20289=CARTESIAN_POINT('Ctrl Pts',(-202.320864073854,94.1974507357616,17.));
#20290=CARTESIAN_POINT('Ctrl Pts',(-202.338369541768,94.1074984825093,17.));
#20291=CARTESIAN_POINT('Ctrl Pts',(-202.360739116816,94.018563693276,17.));
#20292=CARTESIAN_POINT('Ctrl Pts',(-202.38766964512,93.930876392274,17.));
#20293=CARTESIAN_POINT('Ctrl Pts',(-202.415202275748,93.8412286125482,17.));
#20294=CARTESIAN_POINT('Ctrl Pts',(-202.447502301944,93.752884024605,17.));
#20295=CARTESIAN_POINT('Ctrl Pts',(-202.48429995413,93.6660928701058,17.));
#20296=CARTESIAN_POINT('Ctrl Pts',(-202.498927308279,93.631592708318,17.));
#20297=CARTESIAN_POINT('Ctrl Pts',(-202.514265915705,93.5973381158404,17.));
#20298=CARTESIAN_POINT('Ctrl Pts',(-202.53030100434,93.5633453916794,17.));
#20299=CARTESIAN_POINT('Ctrl Pts',(-202.538297772879,93.5463930720939,17.));
#20300=CARTESIAN_POINT('Ctrl Pts',(-202.546469611153,93.5295024211424,17.));
#20301=CARTESIAN_POINT('Ctrl Pts',(-202.554802372669,93.5126998655829,17.));
#20302=CARTESIAN_POINT('Ctrl Pts',(-202.597596782594,93.4264072902949,17.));
#20303=CARTESIAN_POINT('Ctrl Pts',(-202.644686342007,93.3423163357714,17.));
#20304=CARTESIAN_POINT('Ctrl Pts',(-202.69572565248,93.2606735373991,17.));
#20305=CARTESIAN_POINT('Ctrl Pts',(-202.747781901769,93.1774040373738,17.));
#20306=CARTESIAN_POINT('Ctrl Pts',(-202.80394718269,93.0966804560165,17.));
#20307=CARTESIAN_POINT('Ctrl Pts',(-202.863910132442,93.0187715614717,17.));
#20308=CARTESIAN_POINT('Ctrl Pts',(-202.924370593286,92.9402162587798,17.));
#20309=CARTESIAN_POINT('Ctrl Pts',(-202.988692466357,92.8645217114623,17.));
#20310=CARTESIAN_POINT('Ctrl Pts',(-203.056605938085,92.7919828149226,17.));
#20311=CARTESIAN_POINT('Ctrl Pts',(-203.094650995819,92.7513465989163,17.));
#20312=CARTESIAN_POINT('Ctrl Pts',(-203.133824024131,92.7117011149777,17.));
#20313=CARTESIAN_POINT('Ctrl Pts',(-203.174083422688,92.673102348505,17.));
#20314=CARTESIAN_POINT('Ctrl Pts',(-203.185629619105,92.6620324131581,17.));
#20315=CARTESIAN_POINT('Ctrl Pts',(-203.1972651951,92.6510485939825,17.));
#20316=CARTESIAN_POINT('Ctrl Pts',(-203.208989225885,92.6401522676968,17.));
#20317=CARTESIAN_POINT('Ctrl Pts',(-203.219402166174,92.6304744702682,17.));
#20318=CARTESIAN_POINT('Ctrl Pts',(-203.229881653,92.6208687455018,17.));
#20319=CARTESIAN_POINT('Ctrl Pts',(-203.240420864849,92.6113412724527,17.));
#20320=CARTESIAN_POINT('Ctrl Pts',(-203.31613092934,92.5428991906971,17.));
#20321=CARTESIAN_POINT('Ctrl Pts',(-203.39501019773,92.4784087555357,17.));
#20322=CARTESIAN_POINT('Ctrl Pts',(-203.476728217726,92.4181490409495,17.));
#20323=CARTESIAN_POINT('Ctrl Pts',(-203.558538789846,92.3578210774687,17.));
#20324=CARTESIAN_POINT('Ctrl Pts',(-203.643195128873,92.3017325904328,17.));
#20325=CARTESIAN_POINT('Ctrl Pts',(-203.730410869524,92.2501895488276,17.));
#20326=CARTESIAN_POINT('Ctrl Pts',(-203.815807914422,92.1997213259438,17.));
#20327=CARTESIAN_POINT('Ctrl Pts',(-203.903659405823,92.1536102898009,17.));
#20328=CARTESIAN_POINT('Ctrl Pts',(-203.993730337174,92.1121794018575,17.));
#20329=CARTESIAN_POINT('Ctrl Pts',(-204.04409635998,92.08901200461,17.));
#20330=CARTESIAN_POINT('Ctrl Pts',(-204.095156919867,92.0673087145635,17.));
#20331=CARTESIAN_POINT('Ctrl Pts',(-204.146874522078,92.0471322125037,17.));
#20332=CARTESIAN_POINT('Ctrl Pts',(-204.165970757723,92.0396822298796,17.));
#20333=CARTESIAN_POINT('Ctrl Pts',(-204.185156595851,92.0324404568016,17.));
#20334=CARTESIAN_POINT('Ctrl Pts',(-204.204429069408,92.0254062069443,17.));
#20335=CARTESIAN_POINT('Ctrl Pts',(-205.793799282533,92.0307770462543,17.));
#20336=CARTESIAN_POINT('Ctrl Pts',(-205.888625439193,92.0654648779461,17.));
#20337=CARTESIAN_POINT('Ctrl Pts',(-205.981405837457,92.105147830213,17.));
#20338=CARTESIAN_POINT('Ctrl Pts',(-206.071900643333,92.1495042740275,17.));
#20339=CARTESIAN_POINT('Ctrl Pts',(-206.163682037882,92.1944913451757,17.));
#20340=CARTESIAN_POINT('Ctrl Pts',(-206.253113055814,92.2442864444201,17.));
#20341=CARTESIAN_POINT('Ctrl Pts',(-206.339909452525,92.2985947378519,17.));
#20342=CARTESIAN_POINT('Ctrl Pts',(-206.364289257077,92.3138491220152,17.));
#20343=CARTESIAN_POINT('Ctrl Pts',(-206.388460961959,92.3294597884703,17.));
#20344=CARTESIAN_POINT('Ctrl Pts',(-206.412417682282,92.3454206513343,17.));
#20345=CARTESIAN_POINT('Ctrl Pts',(-206.431857110393,92.3583719252173,17.));
#20346=CARTESIAN_POINT('Ctrl Pts',(-206.451157193771,92.3715554798855,17.));
#20347=CARTESIAN_POINT('Ctrl Pts',(-206.470294701023,92.3849541090983,17.));
#20348=CARTESIAN_POINT('Ctrl Pts',(-206.553006045271,92.4428623109673,17.));
#20349=CARTESIAN_POINT('Ctrl Pts',(-206.632761485621,92.5048354140007,17.));
#20350=CARTESIAN_POINT('Ctrl Pts',(-206.709295609939,92.5705745565257,17.));
#20351=CARTESIAN_POINT('Ctrl Pts',(-206.768823569185,92.6217062188,17.));
#20352=CARTESIAN_POINT('Ctrl Pts',(-206.826402117093,92.6751171275772,17.));
#20353=CARTESIAN_POINT('Ctrl Pts',(-206.881888242456,92.7306787828074,17.));
#20354=CARTESIAN_POINT('Ctrl Pts',(-206.912065039079,92.7608966572574,17.));
#20355=CARTESIAN_POINT('Ctrl Pts',(-206.941622633342,92.7917508510965,17.));
#20356=CARTESIAN_POINT('Ctrl Pts',(-206.970535764831,92.8232216127412,17.));
#20357=CARTESIAN_POINT('Ctrl Pts',(-206.98234105479,92.8360711882562,17.));
#20358=CARTESIAN_POINT('Ctrl Pts',(-206.994033802991,92.8490180878463,17.));
#20359=CARTESIAN_POINT('Ctrl Pts',(-207.00560763218,92.8620550677975,17.));
#20360=CARTESIAN_POINT('Ctrl Pts',(-207.071007128224,92.9357222962328,17.));
#20361=CARTESIAN_POINT('Ctrl Pts',(-207.132664441688,93.0123192022955,17.));
#20362=CARTESIAN_POINT('Ctrl Pts',(-207.190334457617,93.0915674062453,17.));
#20363=CARTESIAN_POINT('Ctrl Pts',(-207.247546914657,93.1701868480969,17.));
#20364=CARTESIAN_POINT('Ctrl Pts',(-207.30083553606,93.2514164669213,17.));
#20365=CARTESIAN_POINT('Ctrl Pts',(-207.349914694167,93.3350062931376,17.));
#20366=CARTESIAN_POINT('Ctrl Pts',(-207.397475463616,93.4160100553518,17.));
#20367=CARTESIAN_POINT('Ctrl Pts',(-207.441083386685,93.499230945498,17.));
#20368=CARTESIAN_POINT('Ctrl Pts',(-207.480430624137,93.5844511813323,17.));
#20369=CARTESIAN_POINT('Ctrl Pts',(-207.501046370163,93.6291018061788,17.));
#20370=CARTESIAN_POINT('Ctrl Pts',(-207.520491662325,93.6743013859238,17.));
#20371=CARTESIAN_POINT('Ctrl Pts',(-207.538716459085,93.7200187685398,17.));
#20372=CARTESIAN_POINT('Ctrl Pts',(-207.545013503871,93.7358150712166,17.));
#20373=CARTESIAN_POINT('Ctrl Pts',(-207.551164803887,93.7516731900739,17.));
#20374=CARTESIAN_POINT('Ctrl Pts',(-207.557168177544,93.7675918326183,17.));
#20375=CARTESIAN_POINT('Ctrl Pts',(-207.562729535398,93.7823384189236,17.));
#20376=CARTESIAN_POINT('Ctrl Pts',(-207.568161177558,93.7971297270081,17.));
#20377=CARTESIAN_POINT('Ctrl Pts',(-207.573459278408,93.8119574010363,17.));
#20378=CARTESIAN_POINT('Ctrl Pts',(-207.604693559378,93.8993720709009,17.));
#20379=CARTESIAN_POINT('Ctrl Pts',(-207.631320320326,93.9881282654993,17.));
#20380=CARTESIAN_POINT('Ctrl Pts',(-207.653087336967,94.07800225261,17.));
#20381=CARTESIAN_POINT('Ctrl Pts',(-207.658248256261,94.0993112083491,17.));
#20382=CARTESIAN_POINT('Ctrl Pts',(-207.663135756651,94.1206830429499,17.));
#20383=CARTESIAN_POINT('Ctrl Pts',(-207.667746045347,94.142114835567,17.));
#20384=CARTESIAN_POINT('Ctrl Pts',(-207.687556359468,94.2342068002817,17.));
#20385=CARTESIAN_POINT('Ctrl Pts',(-207.702252352955,94.3274062210526,17.));
#20386=CARTESIAN_POINT('Ctrl Pts',(-207.711945471377,94.4213210251117,17.));
#20387=CARTESIAN_POINT('Ctrl Pts',(-207.722114172796,94.5198436635245,17.));
#20388=CARTESIAN_POINT('Ctrl Pts',(-207.726777055298,94.6191548874199,17.));
#20389=CARTESIAN_POINT('Ctrl Pts',(-207.726004510103,94.7187860623211,17.));
#20390=CARTESIAN_POINT('Ctrl Pts',(-207.725764562221,94.7497309048235,17.));
#20391=CARTESIAN_POINT('Ctrl Pts',(-207.724999859398,94.7807064222678,17.));
#20392=CARTESIAN_POINT('Ctrl Pts',(-207.723711444567,94.8116979686419,17.));
#20393=CARTESIAN_POINT('Ctrl Pts',(-207.723122838063,94.8258563168052,17.));
#20394=CARTESIAN_POINT('Ctrl Pts',(-207.72242484411,94.8400180917865,17.));
#20395=CARTESIAN_POINT('Ctrl Pts',(-207.721618574493,94.8541673752309,17.));
#20396=CARTESIAN_POINT('Ctrl Pts',(-207.716327457255,94.9470215718848,17.));
#20397=CARTESIAN_POINT('Ctrl Pts',(-207.706371961745,95.0394947841683,17.));
#20398=CARTESIAN_POINT('Ctrl Pts',(-207.691879894166,95.131215897366,17.));
#20399=CARTESIAN_POINT('Ctrl Pts',(-207.67741843296,95.2227433010943,17.));
#20400=CARTESIAN_POINT('Ctrl Pts',(-207.658439124386,95.3135227252561,17.));
#20401=CARTESIAN_POINT('Ctrl Pts',(-207.635020244211,95.4031684384919,17.));
#20402=CARTESIAN_POINT('Ctrl Pts',(-207.611996292461,95.4913023953998,17.));
#20403=CARTESIAN_POINT('Ctrl Pts',(-207.584680766522,95.5783413425628,17.));
#20404=CARTESIAN_POINT('Ctrl Pts',(-207.553107669616,95.6638896101273,17.));
#20405=CARTESIAN_POINT('Ctrl Pts',(-207.536805015492,95.708062147942,17.));
#20406=CARTESIAN_POINT('Ctrl Pts',(-207.519366615784,95.7518366999759,17.));
#20407=CARTESIAN_POINT('Ctrl Pts',(-207.500793440028,95.7951546486274,17.));
#20408=CARTESIAN_POINT('Ctrl Pts',(-207.494983232573,95.8087057112732,17.));
#20409=CARTESIAN_POINT('Ctrl Pts',(-207.489061185403,95.8222137843736,17.));
#20410=CARTESIAN_POINT('Ctrl Pts',(-207.48302971481,95.8356715889093,17.));
#20411=CARTESIAN_POINT('Ctrl Pts',(-207.446486009935,95.9172102501051,17.));
#20412=CARTESIAN_POINT('Ctrl Pts',(-207.406052548468,95.9966328231811,17.));
#20413=CARTESIAN_POINT('Ctrl Pts',(-207.361809031731,96.0735940904104,17.));
#20414=CARTESIAN_POINT('Ctrl Pts',(-207.318276147011,96.1493192185477,17.));
#20415=CARTESIAN_POINT('Ctrl Pts',(-207.271054151283,96.2226621614719,17.));
#20416=CARTESIAN_POINT('Ctrl Pts',(-207.22018182407,96.2932611166533,17.));
#20417=CARTESIAN_POINT('Ctrl Pts',(-207.170938066514,96.3615999960239,17.));
#20418=CARTESIAN_POINT('Ctrl Pts',(-207.118273489373,96.4273682047813,17.));
#20419=CARTESIAN_POINT('Ctrl Pts',(-207.062195039505,96.4901984373505,17.));
#20420=CARTESIAN_POINT('Ctrl Pts',(-207.027351919219,96.5292366303853,17.));
#20421=CARTESIAN_POINT('Ctrl Pts',(-206.991190347134,96.5671398225301,17.));
#20422=CARTESIAN_POINT('Ctrl Pts',(-206.953707348215,96.6038107958082,17.));
#20423=CARTESIAN_POINT('Ctrl Pts',(-206.941658583283,96.615598538241,17.));
#20424=CARTESIAN_POINT('Ctrl Pts',(-206.929473251158,96.6272588980258,17.));
#20425=CARTESIAN_POINT('Ctrl Pts',(-206.917153830491,96.638790656604,17.));
#20426=CARTESIAN_POINT('Origin',(-205.,95.,-2.20842344717744));
#20427=CARTESIAN_POINT('Ctrl Pts',(-201.923720806533,95.0022768293025,0.291576552822547));
#20428=CARTESIAN_POINT('Ctrl Pts',(-201.922485619479,95.1502545480464,0.299259877064296));
#20429=CARTESIAN_POINT('Ctrl Pts',(-201.99954223613,96.317136758203,0.359912640907481));
#20430=CARTESIAN_POINT('Ctrl Pts',(-203.493269023741,98.307102300781,0.473534844352101));
#20431=CARTESIAN_POINT('Ctrl Pts',(-206.963865970602,98.0574884319591,0.632443163156409));
#20432=CARTESIAN_POINT('Ctrl Pts',(-208.633932648393,95.0051905167663,0.791351481960714));
#20433=CARTESIAN_POINT('Ctrl Pts',(-206.972489133437,91.9479467192658,0.950259800765022));
#20434=CARTESIAN_POINT('Ctrl Pts',(-203.50267093535,91.6888818401662,1.10916811956933));
#20435=CARTESIAN_POINT('Ctrl Pts',(-202.001246091317,93.6767401604291,1.22294037025517));
#20436=CARTESIAN_POINT('Ctrl Pts',(-201.922516654998,94.8467460489523,1.28374318133958));
#20437=CARTESIAN_POINT('Ctrl Pts',(-201.923792939525,94.9976530037673,1.29157655282255));
#20438=CARTESIAN_POINT('Ctrl Pts',(-201.929615821727,94.9968993793473,0.208423447177457));
#20439=CARTESIAN_POINT('Ctrl Pts',(-201.934957629034,95.7021699935174,0.244887843987842));
#20440=CARTESIAN_POINT('Ctrl Pts',(-202.525017792303,97.4423245699489,0.334321680399662));
#20441=CARTESIAN_POINT('Ctrl Pts',(-205.417647311761,98.6092821234889,0.476724956412918));
#20442=CARTESIAN_POINT('Ctrl Pts',(-208.260128930045,96.6049848945777,0.635633275217225));
#20443=CARTESIAN_POINT('Ctrl Pts',(-208.114979909401,93.1280855192232,0.794541594021532));
#20444=CARTESIAN_POINT('Ctrl Pts',(-205.113462578231,91.3679026833885,0.953449912825839));
#20445=CARTESIAN_POINT('Ctrl Pts',(-202.417551634193,92.7304286396575,1.09141053054448));
#20446=CARTESIAN_POINT('Ctrl Pts',(-201.933584023895,94.3813001345165,1.17640170866169));
#20447=CARTESIAN_POINT('Ctrl Pts',(-201.930545984431,95.0016532623852,1.20842344717746));
#20448=CARTESIAN_POINT('Ctrl Pts',(-206.913465996665,96.6359872033749,0.));
#20449=CARTESIAN_POINT('Ctrl Pts',(-207.457950030113,95.9991535645904,0.0529694396014356));
#20450=CARTESIAN_POINT('Ctrl Pts',(-207.850594391536,94.1490681946565,0.158908318804307));
#20451=CARTESIAN_POINT('Ctrl Pts',(-205.826561431148,92.1388044389514,0.317816637608613));
#20452=CARTESIAN_POINT('Ctrl Pts',(-203.043475148172,92.7574356177759,0.47672495641292));
#20453=CARTESIAN_POINT('Ctrl Pts',(-202.054677609388,95.4292087310772,0.635633275217227));
#20454=CARTESIAN_POINT('Ctrl Pts',(-203.765838544743,97.7088433519493,0.794541594021533));
#20455=CARTESIAN_POINT('Ctrl Pts',(-206.608600156496,97.5043849446744,0.953449912825841));
#20456=CARTESIAN_POINT('Ctrl Pts',(-207.976549680276,95.0042515457814,1.11235823163015));
#20457=CARTESIAN_POINT('Ctrl Pts',(-206.615663378372,92.5000669808854,1.27126655043445));
#20458=CARTESIAN_POINT('Ctrl Pts',(-203.773539638765,92.2878672629311,1.43017486923876));
#20459=CARTESIAN_POINT('Ctrl Pts',(-202.055828455909,94.5620846373259,1.58908318804307));
#20460=CARTESIAN_POINT('Ctrl Pts',(-203.037297256324,97.2377952804476,1.74799150684737));
#20461=CARTESIAN_POINT('Ctrl Pts',(-205.818151727977,97.8619118255793,1.90689982565168));
#20462=CARTESIAN_POINT('Ctrl Pts',(-207.848933001711,95.8622636572055,2.06580814445599));
#20463=CARTESIAN_POINT('Ctrl Pts',(-207.267844746755,93.0720998408888,2.2247164632603));
#20464=CARTESIAN_POINT('Ctrl Pts',(-204.607621579145,92.0494142928463,2.3836247820646));
#20465=CARTESIAN_POINT('Ctrl Pts',(-202.307126657076,93.7317922834607,2.54253310086891));
#20466=CARTESIAN_POINT('Ctrl Pts',(-202.47542787224,96.5768491563952,2.70144141967321));
#20467=CARTESIAN_POINT('Ctrl Pts',(-204.958228619701,97.9762682393428,2.86034973847752));
#20468=CARTESIAN_POINT('Ctrl Pts',(-207.479324891018,96.6470779176025,3.01925805728183));
#20469=CARTESIAN_POINT('Ctrl Pts',(-207.727403818342,93.8078649448984,3.17816637608613));
#20470=CARTESIAN_POINT('Ctrl Pts',(-205.475029406128,92.0615880786317,3.33707469489044));
#20471=CARTESIAN_POINT('Ctrl Pts',(-202.787153344895,93.0092144139677,3.49598301369475));
#20472=CARTESIAN_POINT('Ctrl Pts',(-202.127990363946,95.7819707268259,3.65489133249905));
#20473=CARTESIAN_POINT('Ctrl Pts',(-204.101853717757,97.8378250158782,3.81379965130336));
#20474=CARTESIAN_POINT('Ctrl Pts',(-206.899127544596,97.2919930488229,3.97270797010767));
#20475=CARTESIAN_POINT('Ctrl Pts',(-207.955302464772,94.6448874714171,4.13161628891197));
#20476=CARTESIAN_POINT('Ctrl Pts',(-206.302089116017,92.3233450913524,4.29052460771628));
#20477=CARTESIAN_POINT('Ctrl Pts',(-203.455135018895,92.4557300150421,4.44943292652059));
#20478=CARTESIAN_POINT('Ctrl Pts',(-202.024495869805,94.9206732241979,4.60834124532489));
#20479=CARTESIAN_POINT('Ctrl Pts',(-203.321765650688,97.4583423347725,4.7672495641292));
#20480=CARTESIAN_POINT('Ctrl Pts',(-206.15762192574,97.7422306692202,4.9261578829335));
#20481=CARTESIAN_POINT('Ctrl Pts',(-207.932183357775,95.5120725754678,5.08506620173781));
#20482=CARTESIAN_POINT('Ctrl Pts',(-207.018551859809,92.8124520678579,5.24397452054212));
#20483=CARTESIAN_POINT('Ctrl Pts',(-204.254334577707,92.1183510546639,5.40288283934642));
#20484=CARTESIAN_POINT('Ctrl Pts',(-202.173735020615,94.06611358696,5.56179115815073));
#20485=CARTESIAN_POINT('Ctrl Pts',(-202.684223608044,96.8700527448756,5.72069947695504));
#20486=CARTESIAN_POINT('Ctrl Pts',(-205.317790108664,97.9595484474823,5.87960779575935));
#20487=CARTESIAN_POINT('Ctrl Pts',(-207.660010189536,96.3357632116982,6.03851611456365));
#20488=CARTESIAN_POINT('Ctrl Pts',(-207.563562659025,93.4873651929785,6.19742443336796));
#20489=CARTESIAN_POINT('Ctrl Pts',(-205.11686953513,92.0257338589296,6.35633275217227));
#20490=CARTESIAN_POINT('Ctrl Pts',(-202.563031727655,93.2908764802563,6.51524107097657));
#20491=CARTESIAN_POINT('Ctrl Pts',(-202.243379194775,96.1229244419638,6.67414938978088));
#20492=CARTESIAN_POINT('Ctrl Pts',(-204.450965805945,97.9254878259732,6.83305770858519));
#20493=CARTESIAN_POINT('Ctrl Pts',(-207.161900829783,97.045996668703,6.99196602738949));
#20494=CARTESIAN_POINT('Ctrl Pts',(-207.890829335995,94.2907586332476,7.15087434619381));
#20495=CARTESIAN_POINT('Ctrl Pts',(-205.969477817168,92.1857451557867,7.3097826649981));
#20496=CARTESIAN_POINT('Ctrl Pts',(-203.159319871215,92.660809065156,7.46869098380242));
#20497=CARTESIAN_POINT('Ctrl Pts',(-202.036676894431,95.2804170789368,7.62759930260672));
#20498=CARTESIAN_POINT('Ctrl Pts',(-203.630775420383,97.6429418489121,7.78650762141103));
#20499=CARTESIAN_POINT('Ctrl Pts',(-206.480163737388,97.5824470714193,7.94541594021534));
#20500=CARTESIAN_POINT('Ctrl Pts',(-207.972554483439,95.1543936823264,8.10432425901963));
#20501=CARTESIAN_POINT('Ctrl Pts',(-206.739740502701,92.5847938909029,8.26323257782395));
#20502=CARTESIAN_POINT('Ctrl Pts',(-203.911951873806,92.2294280660402,8.42214089662825));
#20503=CARTESIAN_POINT('Ctrl Pts',(-202.081673606117,94.4140916241222,8.58104921543256));
#20504=CARTESIAN_POINT('Ctrl Pts',(-202.926884358809,97.1359094326323,8.73995753423688));
#20505=CARTESIAN_POINT('Ctrl Pts',(-205.67270436056,97.899549345923,8.89886585304117));
#20506=CARTESIAN_POINT('Ctrl Pts',(-207.801796523227,96.0049148265353,9.05777417184549));
#20507=CARTESIAN_POINT('Ctrl Pts',(-207.3622329485,93.188985625905,9.21668249064978));
#20508=CARTESIAN_POINT('Ctrl Pts',(-204.757000608778,92.033374162112,9.3755908094541));
#20509=CARTESIAN_POINT('Ctrl Pts',(-202.374547394973,93.5975321091309,9.5344991282584));
#20510=CARTESIAN_POINT('Ctrl Pts',(-202.399079785317,96.4474569434051,9.69340744706271));
#20511=CARTESIAN_POINT('Ctrl Pts',(-204.808106758534,97.9703694298923,9.85231576586701));
#20512=CARTESIAN_POINT('Ctrl Pts',(-207.393059310776,96.7700804222594,10.0112240846713));
#20513=CARTESIAN_POINT('Ctrl Pts',(-207.784081833628,93.9470014673218,10.1701324034756));
#20514=CARTESIAN_POINT('Ctrl Pts',(-205.622689248516,92.0892997979969,10.3290407222799));
#20515=CARTESIAN_POINT('Ctrl Pts',(-202.890422120034,92.9000955415738,10.4879490410842));
#20516=CARTESIAN_POINT('Ctrl Pts',(-202.092192413589,95.6360602224381,10.6468573598885));
#20517=CARTESIAN_POINT('Ctrl Pts',(-203.959808202401,97.7888920004845,10.8057656786928));
#20518=CARTESIAN_POINT('Ctrl Pts',(-206.781060205243,97.3848987633562,10.9646739974972));
#20519=CARTESIAN_POINT('Ctrl Pts',(-207.96945611846,94.7944569955031,11.1235823163015));
#20520=CARTESIAN_POINT('Ctrl Pts',(-206.43548785127,92.3924547568613,11.2824906351058));
#20521=CARTESIAN_POINT('Ctrl Pts',(-203.585480366186,92.3810208531348,11.4413989539101));
#20522=CARTESIAN_POINT('Ctrl Pts',(-202.03228867159,94.7706377594659,11.6003072727144));
#20523=CARTESIAN_POINT('Ctrl Pts',(-203.199861553383,97.3705314043844,11.7592155915187));
#20524=CARTESIAN_POINT('Ctrl Pts',(-206.017781243261,97.7971483527026,11.918123910323));
#20525=CARTESIAN_POINT('Ctrl Pts',(-207.902610464846,95.6593709544117,12.0770322291273));
#20526=CARTESIAN_POINT('Ctrl Pts',(-207.126358854139,92.9170896347696,12.2359405479316));
#20527=CARTESIAN_POINT('Ctrl Pts',(-204.400685211829,92.0843972577109,12.3948488667359));
#20528=CARTESIAN_POINT('Ctrl Pts',(-202.2244566689,93.9246968876966,12.5537571855402));
#20529=CARTESIAN_POINT('Ctrl Pts',(-202.592815230243,96.7508223925955,12.7126655043445));
#20530=CARTESIAN_POINT('Ctrl Pts',(-205.168053883906,97.9718134965553,12.8715738231488));
#20531=CARTESIAN_POINT('Ctrl Pts',(-207.589222615081,96.4682792021923,13.0304821419532));
#20532=CARTESIAN_POINT('Ctrl Pts',(-207.636620992011,93.6186429459658,13.1893904607575));
#20533=CARTESIAN_POINT('Ctrl Pts',(-205.266794712318,92.0354193976255,13.3482987795618));
#20534=CARTESIAN_POINT('Ctrl Pts',(-202.652374022519,93.1700902112655,13.5072070983661));
#20535=CARTESIAN_POINT('Ctrl Pts',(-202.190230589454,95.9824018662228,13.6661154171704));
#20536=CARTESIAN_POINT('Ctrl Pts',(-204.30405234878,97.8940584713035,13.8250237359747));
#20537=CARTESIAN_POINT('Ctrl Pts',(-207.055911134185,97.1524746141731,13.983932054779));
#20538=CARTESIAN_POINT('Ctrl Pts',(-207.922933574598,94.4375260926946,14.1428403735833));
#20539=CARTESIAN_POINT('Ctrl Pts',(-206.110243173882,92.2382473541743,14.3017486923876));
#20540=CARTESIAN_POINT('Ctrl Pts',(-203.279694258837,92.5709125915988,14.4606570111919));
#20541=CARTESIAN_POINT('Ctrl Pts',(-202.026302381485,95.1305379788577,14.6195653299962));
#20542=CARTESIAN_POINT('Ctrl Pts',(-203.499163323573,97.5704876821364,14.7784736488005));
#20543=CARTESIAN_POINT('Ctrl Pts',(-206.347974392351,97.6538428510329,14.9373819676048));
#20544=CARTESIAN_POINT('Ctrl Pts',(-207.960977942727,95.3041848805748,15.0962902864091));
#20545=CARTESIAN_POINT('Ctrl Pts',(-206.859389309675,92.6756529394601,15.2551986052134));
#20546=CARTESIAN_POINT('Ctrl Pts',(-204.053134786262,92.1780577939307,15.4141069240178));
#20547=CARTESIAN_POINT('Ctrl Pts',(-202.114952716846,94.2675848505183,15.573015242822));
#20548=CARTESIAN_POINT('Ctrl Pts',(-202.821755934838,97.0285878680713,15.7319235616264));
#20549=CARTESIAN_POINT('Ctrl Pts',(-205.525536181393,97.9297919249001,15.8908318804307));
#20550=CARTESIAN_POINT('Ctrl Pts',(-207.747537161995,96.1450208713066,16.049740199235));
#20551=CARTESIAN_POINT('Ctrl Pts',(-207.450572136011,93.3104550077017,16.2086485180393));
#20552=CARTESIAN_POINT('Ctrl Pts',(-204.907062940556,92.0249535940473,16.3675568368436));
#20553=CARTESIAN_POINT('Ctrl Pts',(-202.448523832117,93.4667171925034,16.5264651556479));
#20554=CARTESIAN_POINT('Ctrl Pts',(-202.32963244197,96.3146411010228,16.6853734744522));
#20555=CARTESIAN_POINT('Ctrl Pts',(-204.657905606643,97.9563585591527,16.8442817932565));
#20556=CARTESIAN_POINT('Ctrl Pts',(-207.301870809105,96.8897181314193,17.0031901120608));
#20557=CARTESIAN_POINT('Ctrl Pts',(-207.831183483043,94.0865595762447,17.1620984308651));
#20558=CARTESIAN_POINT('Ctrl Pts',(-206.459639356019,92.7843106836636,17.268037310068));
#20559=CARTESIAN_POINT('Ctrl Pts',(-205.650199997975,92.567913197965,17.3210067496694));
#20560=CARTESIAN_POINT('Ctrl Pts',(-207.054331550342,96.7564253212268,-0.107002249889811));
#20561=CARTESIAN_POINT('Ctrl Pts',(-207.63889941333,96.0727092589846,-0.0540328102883751));
#20562=CARTESIAN_POINT('Ctrl Pts',(-208.060449470211,94.086424290814,0.0519060689144962));
#20563=CARTESIAN_POINT('Ctrl Pts',(-205.887411236606,91.9281689233017,0.210814387718803));
#20564=CARTESIAN_POINT('Ctrl Pts',(-202.899439687382,92.5923424967542,0.369722706523109));
#20565=CARTESIAN_POINT('Ctrl Pts',(-201.837848844186,95.4608062225673,0.528631025327416));
#20566=CARTESIAN_POINT('Ctrl Pts',(-203.674982037743,97.9082630015598,0.687539344131723));
#20567=CARTESIAN_POINT('Ctrl Pts',(-206.727022094531,97.6887527737694,0.84644766293603));
#20568=CARTESIAN_POINT('Ctrl Pts',(-208.195677336315,95.0045645361097,1.00535598174034));
#20569=CARTESIAN_POINT('Ctrl Pts',(-206.734605296727,92.3160268936789,1.16426430054464));
#20570=CARTESIAN_POINT('Ctrl Pts',(-203.68325007096,92.0882054553427,1.32317261934895));
#20571=CARTESIAN_POINT('Ctrl Pts',(-201.839084413736,94.5298461809676,1.48208093815326));
#20572=CARTESIAN_POINT('Ctrl Pts',(-202.892806991447,97.4025373097,1.64098925695756));
#20573=CARTESIAN_POINT('Ctrl Pts',(-205.878382427845,98.0726000711963,1.79989757576187));
#20574=CARTESIAN_POINT('Ctrl Pts',(-208.058665772177,95.9257417894009,1.95880589456617));
#20575=CARTESIAN_POINT('Ctrl Pts',(-207.434798957837,92.9301716729358,2.11771421337049));
#20576=CARTESIAN_POINT('Ctrl Pts',(-204.578735461701,91.8321980527698,2.27662253217479));
#20577=CARTESIAN_POINT('Ctrl Pts',(-202.108882687706,93.638429358549,2.4355308509791));
#20578=CARTESIAN_POINT('Ctrl Pts',(-202.289573902954,96.6929336490738,2.5944391697834));
#20579=CARTESIAN_POINT('Ctrl Pts',(-204.955153493922,98.1953751762611,2.75334748858771));
#20580=CARTESIAN_POINT('Ctrl Pts',(-207.661847848901,96.7683325117351,2.91225580739201));
#20581=CARTESIAN_POINT('Ctrl Pts',(-207.928189852503,93.7201023377304,3.07116412619633));
#20582=CARTESIAN_POINT('Ctrl Pts',(-205.510000124407,91.8452680484058,3.23007244500063));
#20583=CARTESIAN_POINT('Ctrl Pts',(-202.624247983725,92.8626567461976,3.38898076380494));
#20584=CARTESIAN_POINT('Ctrl Pts',(-201.916558737644,95.8395378534879,3.54788908260924));
#20585=CARTESIAN_POINT('Ctrl Pts',(-204.03573397821,98.0467400385633,3.70679740141355));
#20586=CARTESIAN_POINT('Ctrl Pts',(-207.038937530004,97.4607250097823,3.86570572021785));
#20587=CARTESIAN_POINT('Ctrl Pts',(-208.172865943145,94.6187447947018,4.02461403902216));
#20588=CARTESIAN_POINT('Ctrl Pts',(-206.397946322042,92.1262950907953,4.18352235782647));
#20589=CARTESIAN_POINT('Ctrl Pts',(-203.341405137465,92.2684259287611,4.34243067663078));
#20590=CARTESIAN_POINT('Ctrl Pts',(-201.80544518508,94.9148333450394,4.50133899543508));
#20591=CARTESIAN_POINT('Ctrl Pts',(-203.198217382139,97.6393205986763,4.66024731423939));
#20592=CARTESIAN_POINT('Ctrl Pts',(-206.242843745099,97.9441082265968,4.8191556330437));
#20593=CARTESIAN_POINT('Ctrl Pts',(-208.148044853561,95.5497703380577,4.978063951848));
#20594=CARTESIAN_POINT('Ctrl Pts',(-207.167153625324,92.651409148259,5.13697227065232));
#20595=CARTESIAN_POINT('Ctrl Pts',(-204.199440175218,91.9062098016209,5.29588058945661));
#20596=CARTESIAN_POINT('Ctrl Pts',(-201.965671024781,93.9973627302039,5.45478890826093));
#20597=CARTESIAN_POINT('Ctrl Pts',(-202.513740764756,97.0077223014663,5.61369722706523));
#20598=CARTESIAN_POINT('Ctrl Pts',(-205.341185183198,98.1774245066414,5.77260554586953));
#20599=CARTESIAN_POINT('Ctrl Pts',(-207.85583483904,96.4340994375446,5.93151386467385));
#20600=CARTESIAN_POINT('Ctrl Pts',(-207.752287033526,93.3760080327397,6.09042218347815));
#20601=CARTESIAN_POINT('Ctrl Pts',(-205.125473237418,91.8067743124966,6.24933050228246));
#20602=CARTESIAN_POINT('Ctrl Pts',(-202.383626979634,93.1650542125334,6.40823882108677));
#20603=CARTESIAN_POINT('Ctrl Pts',(-202.040442264261,96.2055919017098,6.56714713989107));
#20604=CARTESIAN_POINT('Ctrl Pts',(-204.410547002649,98.1408564100502,6.72605545869538));
#20605=CARTESIAN_POINT('Ctrl Pts',(-207.321055660813,97.1966188663592,6.88496377749968));
#20606=CARTESIAN_POINT('Ctrl Pts',(-208.103646431104,94.2385456971451,7.04387209630399));
#20607=CARTESIAN_POINT('Ctrl Pts',(-206.040848842172,91.978565322171,7.2027804151083));
#20608=CARTESIAN_POINT('Ctrl Pts',(-203.02381266809,92.4886024898798,7.36168873391261));
#20609=CARTESIAN_POINT('Ctrl Pts',(-201.818522952465,95.3010608254961,7.52059705271691));
#20610=CARTESIAN_POINT('Ctrl Pts',(-203.529975835309,97.8375099611922,7.67950537152122));
#20611=CARTESIAN_POINT('Ctrl Pts',(-206.589130442186,97.7725616787294,7.83841369032553));
#20612=CARTESIAN_POINT('Ctrl Pts',(-208.191388021049,95.1657598375562,7.99732200912982));
#20613=CARTESIAN_POINT('Ctrl Pts',(-206.867816731698,92.4069912299749,8.15623032793414));
#20614=CARTESIAN_POINT('Ctrl Pts',(-203.831851938928,92.0254640812297,8.31513864673844));
#20615=CARTESIAN_POINT('Ctrl Pts',(-201.866832232399,94.3709582170401,8.47404696554276));
#20616=CARTESIAN_POINT('Ctrl Pts',(-202.774265716439,97.2931508287983,8.63295528434705));
#20617=CARTESIAN_POINT('Ctrl Pts',(-205.722227515074,98.1130083907867,8.79186360315136));
#20618=CARTESIAN_POINT('Ctrl Pts',(-208.008059200078,96.0788946535532,8.95077192195567));
#20619=CARTESIAN_POINT('Ctrl Pts',(-207.536135830906,93.0556623565245,9.10968024075997));
#20620=CARTESIAN_POINT('Ctrl Pts',(-204.739111477825,91.8149770795743,9.26858855956429));
#20621=CARTESIAN_POINT('Ctrl Pts',(-202.181266805977,93.4942852177277,9.42749687836859));
#20622=CARTESIAN_POINT('Ctrl Pts',(-202.207605222011,96.5540158392056,9.5864051971729));
#20623=CARTESIAN_POINT('Ctrl Pts',(-204.793979960486,98.1890421082134,9.7453135159772));
#20624=CARTESIAN_POINT('Ctrl Pts',(-207.569231568544,96.9003902156756,9.90422183478152));
#20625=CARTESIAN_POINT('Ctrl Pts',(-207.989040390331,93.8694818136749,10.0631301535858));
#20626=CARTESIAN_POINT('Ctrl Pts',(-205.668530390149,91.8750198493291,10.2220384723901));
#20627=CARTESIAN_POINT('Ctrl Pts',(-202.735119200304,92.7455047598612,10.3809467911944));
#20628=CARTESIAN_POINT('Ctrl Pts',(-201.878125413517,95.6828857085255,10.5398551099987));
#20629=CARTESIAN_POINT('Ctrl Pts',(-203.88323135507,97.9942046720859,10.698763428803));
#20630=CARTESIAN_POINT('Ctrl Pts',(-206.912178308403,97.5604702578846,10.8576717476073));
#20631=CARTESIAN_POINT('Ctrl Pts',(-208.188061560614,94.7793253291012,11.0165800664117));
#20632=CARTESIAN_POINT('Ctrl Pts',(-206.541165606359,92.2004924721629,11.175488385216));
#20633=CARTESIAN_POINT('Ctrl Pts',(-203.481346249483,92.1882168272285,11.3343967040203));
#20634=CARTESIAN_POINT('Ctrl Pts',(-201.813811677403,94.7537525683722,11.4933050228246));
#20635=CARTESIAN_POINT('Ctrl Pts',(-203.067338948111,97.5450452025753,11.6522133416289));
#20636=CARTESIAN_POINT('Ctrl Pts',(-206.092708270239,98.0030688405018,11.8111216604332));
#20637=CARTESIAN_POINT('Ctrl Pts',(-208.116294863185,95.7079125301353,11.9700299792375));
#20638=CARTESIAN_POINT('Ctrl Pts',(-207.282897155748,92.7637499243336,12.1289382980418));
#20639=CARTESIAN_POINT('Ctrl Pts',(-204.356564851388,91.8697563937965,12.2878466168461));
#20640=CARTESIAN_POINT('Ctrl Pts',(-202.020126699738,93.8455352153444,12.4467549356504));
#20641=CARTESIAN_POINT('Ctrl Pts',(-202.415603084333,96.8797144482438,12.6056632544547));
#20642=CARTESIAN_POINT('Ctrl Pts',(-205.180425675956,98.1905924841865,12.764571573259));
#20643=CARTESIAN_POINT('Ctrl Pts',(-207.779836024414,96.5763709911918,12.9234798920633));
#20644=CARTESIAN_POINT('Ctrl Pts',(-207.830723775401,93.5169501923025,13.0823882108676));
#20645=CARTESIAN_POINT('Ctrl Pts',(-205.286435607392,91.8171728812507,13.241296529672));
#20646=CARTESIAN_POINT('Ctrl Pts',(-202.479546476212,93.0353758991123,13.4002048484763));
#20647=CARTESIAN_POINT('Ctrl Pts',(-201.983380964526,96.0547243339646,13.5591131672806));
#20648=CARTESIAN_POINT('Ctrl Pts',(-204.252818069524,98.1071132889195,13.7180214860849));
#20649=CARTESIAN_POINT('Ctrl Pts',(-207.207263215033,97.3109355059944,13.8769298048892));
#20650=CARTESIAN_POINT('Ctrl Pts',(-208.138114119778,94.3961178844905,14.0358381236935));
#20651=CARTESIAN_POINT('Ctrl Pts',(-206.191977063942,92.0349326277818,14.1947464424978));
#20652=CARTESIAN_POINT('Ctrl Pts',(-203.153048778256,92.3920880170776,14.3536547613021));
#20653=CARTESIAN_POINT('Ctrl Pts',(-201.80738468855,95.1401479247359,14.5125630801064));
#20654=CARTESIAN_POINT('Ctrl Pts',(-203.388674718198,97.7597218630391,14.6714713989107));
#20655=CARTESIAN_POINT('Ctrl Pts',(-206.447209580983,97.8492134733665,14.830379717715));
#20656=CARTESIAN_POINT('Ctrl Pts',(-208.178959238477,95.3265783653281,14.9892880365193));
#20657=CARTESIAN_POINT('Ctrl Pts',(-206.996273845415,92.5045391406305,15.1481963553236));
#20658=CARTESIAN_POINT('Ctrl Pts',(-203.983428456062,91.970312032054,15.3071046741279));
#20659=CARTESIAN_POINT('Ctrl Pts',(-201.902561284944,94.21366590671,15.4660129929322));
#20660=CARTESIAN_POINT('Ctrl Pts',(-202.661397947386,97.1779284645159,15.6249213117365));
#20661=CARTESIAN_POINT('Ctrl Pts',(-205.564225107822,98.1454773681632,15.7838296305409));
#20662=CARTESIAN_POINT('Ctrl Pts',(-207.949805372795,96.229315026149,15.9427379493452));
#20663=CARTESIAN_POINT('Ctrl Pts',(-207.630978373366,93.1860740721548,16.1016462681495));
#20664=CARTESIAN_POINT('Ctrl Pts',(-204.900221099437,91.8059366060685,16.2605545869538));
#20665=CARTESIAN_POINT('Ctrl Pts',(-202.260689241009,93.3538399676152,16.4194629057581));
#20666=CARTESIAN_POINT('Ctrl Pts',(-202.133045303636,96.4114223591716,16.5783712245624));
#20667=CARTESIAN_POINT('Ctrl Pts',(-204.632721299102,98.1739997850896,16.7372795433667));
#20668=CARTESIAN_POINT('Ctrl Pts',(-207.471329951093,97.0288354145798,16.896187862171));
#20669=CARTESIAN_POINT('Ctrl Pts',(-208.039609569315,94.0193139124767,17.0550961809753));
#20670=CARTESIAN_POINT('Ctrl Pts',(-206.56709509676,92.6211960514381,17.1610350601782));
#20671=CARTESIAN_POINT('Ctrl Pts',(-205.698066426161,92.3888678140614,17.2140044997796));
#20672=CARTESIAN_POINT('Ctrl Pts',(-207.195197104019,96.8768634390787,-0.214004499779621));
#20673=CARTESIAN_POINT('Ctrl Pts',(-207.819848796546,96.1462649533789,-0.161035060178185));
#20674=CARTESIAN_POINT('Ctrl Pts',(-208.270304548887,94.0237803869714,-0.0550961809753146));
#20675=CARTESIAN_POINT('Ctrl Pts',(-205.948261042063,91.7175334076522,0.103812137828992));
#20676=CARTESIAN_POINT('Ctrl Pts',(-202.755404226592,92.4272493757325,0.262720456633299));
#20677=CARTESIAN_POINT('Ctrl Pts',(-201.621020078985,95.4924037140574,0.421628775437605));
#20678=CARTESIAN_POINT('Ctrl Pts',(-203.584125530742,98.1076826511703,0.580537094241912));
#20679=CARTESIAN_POINT('Ctrl Pts',(-206.845444032567,97.8731206028643,0.739445413046219));
#20680=CARTESIAN_POINT('Ctrl Pts',(-208.414804992354,95.004877526438,0.898353731850526));
#20681=CARTESIAN_POINT('Ctrl Pts',(-206.853547215082,92.1319868064724,1.05726205065483));
#20682=CARTESIAN_POINT('Ctrl Pts',(-203.592960503155,91.8885436477545,1.21617036945914));
#20683=CARTESIAN_POINT('Ctrl Pts',(-201.622340371563,94.4976077246091,1.37507868826345));
#20684=CARTESIAN_POINT('Ctrl Pts',(-202.74831672657,97.5672793389525,1.53398700706775));
#20685=CARTESIAN_POINT('Ctrl Pts',(-205.938613127714,98.2832883168132,1.69289532587206));
#20686=CARTESIAN_POINT('Ctrl Pts',(-208.268398542644,95.9892199215965,1.85180364467636));
#20687=CARTESIAN_POINT('Ctrl Pts',(-207.601753168919,92.7882435049825,2.01071196348067));
#20688=CARTESIAN_POINT('Ctrl Pts',(-204.549849344257,91.6149818126935,2.16962028228498));
#20689=CARTESIAN_POINT('Ctrl Pts',(-201.910638718336,93.5450664336372,2.32852860108929));
#20690=CARTESIAN_POINT('Ctrl Pts',(-202.103719933668,96.8090181417526,2.48743691989359));
#20691=CARTESIAN_POINT('Ctrl Pts',(-204.952078368144,98.4144821131792,2.6463452386979));
#20692=CARTESIAN_POINT('Ctrl Pts',(-207.844370806783,96.8895871058678,2.8052535575022));
#20693=CARTESIAN_POINT('Ctrl Pts',(-208.128975886664,93.6323397305624,2.96416187630651));
#20694=CARTESIAN_POINT('Ctrl Pts',(-205.544970842687,91.6289480181799,3.12307019511082));
#20695=CARTESIAN_POINT('Ctrl Pts',(-202.461342622555,92.7160990784275,3.28197851391512));
#20696=CARTESIAN_POINT('Ctrl Pts',(-201.705127111342,95.89710498015,3.44088683271943));
#20697=CARTESIAN_POINT('Ctrl Pts',(-203.969614238663,98.2556550612482,3.59979515152374));
#20698=CARTESIAN_POINT('Ctrl Pts',(-207.178747515412,97.6294569707416,3.75870347032805));
#20699=CARTESIAN_POINT('Ctrl Pts',(-208.390429421518,94.5926021179864,3.91761178913235));
#20700=CARTESIAN_POINT('Ctrl Pts',(-206.493803528068,91.9292450902381,4.07652010793666));
#20701=CARTESIAN_POINT('Ctrl Pts',(-203.227675256036,92.0811218424802,4.23542842674097));
#20702=CARTESIAN_POINT('Ctrl Pts',(-201.586394500355,94.9089934658807,4.39433674554527));
#20703=CARTESIAN_POINT('Ctrl Pts',(-203.074669113589,97.8202988625801,4.55324506434958));
#20704=CARTESIAN_POINT('Ctrl Pts',(-206.328065564458,98.1459857839733,4.71215338315389));
#20705=CARTESIAN_POINT('Ctrl Pts',(-208.363906349347,95.5874681006477,4.8710617019582));
#20706=CARTESIAN_POINT('Ctrl Pts',(-207.31575539084,92.49036622866,5.0299700207625));
#20707=CARTESIAN_POINT('Ctrl Pts',(-204.14454577273,91.6940685485779,5.18887833956681));
#20708=CARTESIAN_POINT('Ctrl Pts',(-201.757607028947,93.9286118734479,5.34778665837111));
#20709=CARTESIAN_POINT('Ctrl Pts',(-202.343257921469,97.1453918580569,5.50669497717542));
#20710=CARTESIAN_POINT('Ctrl Pts',(-205.364580257732,98.3953005658008,5.66560329597973));
#20711=CARTESIAN_POINT('Ctrl Pts',(-208.051659488544,96.5324356633908,5.82451161478403));
#20712=CARTESIAN_POINT('Ctrl Pts',(-207.941011408027,93.2646508725009,5.98341993358834));
#20713=CARTESIAN_POINT('Ctrl Pts',(-205.134076939706,91.5878147660635,6.14232825239264));
#20714=CARTESIAN_POINT('Ctrl Pts',(-202.204222231614,93.0392319448105,6.30123657119695));
#20715=CARTESIAN_POINT('Ctrl Pts',(-201.837505333748,96.2882593614559,6.46014489000126));
#20716=CARTESIAN_POINT('Ctrl Pts',(-204.370128199352,98.3562249941271,6.61905320880556));
#20717=CARTESIAN_POINT('Ctrl Pts',(-207.480210491844,97.3472410640154,6.77796152760988));
#20718=CARTESIAN_POINT('Ctrl Pts',(-208.316463526213,94.1863327610426,6.93686984641418));
#20719=CARTESIAN_POINT('Ctrl Pts',(-206.112219867177,91.7713854885552,7.09577816521849));
#20720=CARTESIAN_POINT('Ctrl Pts',(-202.888305464964,92.3163959146037,7.25468648402279));
#20721=CARTESIAN_POINT('Ctrl Pts',(-201.600369010499,95.3217045720554,7.4135948028271));
#20722=CARTESIAN_POINT('Ctrl Pts',(-203.429176250236,98.0320780734722,7.5725031216314));
#20723=CARTESIAN_POINT('Ctrl Pts',(-206.698097146984,97.9626762860395,7.73141144043571));
#20724=CARTESIAN_POINT('Ctrl Pts',(-208.410221558658,95.177125992786,7.89031975924002));
#20725=CARTESIAN_POINT('Ctrl Pts',(-206.995892960696,92.229188569047,8.04922807804433));
#20726=CARTESIAN_POINT('Ctrl Pts',(-203.751752004051,91.8215000964192,8.20813639684864));
#20727=CARTESIAN_POINT('Ctrl Pts',(-201.651990858682,94.3278248099579,8.36704471565293));
#20728=CARTESIAN_POINT('Ctrl Pts',(-202.621647074068,97.4503922249643,8.52595303445725));
#20729=CARTESIAN_POINT('Ctrl Pts',(-205.771750669589,98.3264674356504,8.68486135326155));
#20730=CARTESIAN_POINT('Ctrl Pts',(-208.214321876929,96.1528744805713,8.84376967206586));
#20731=CARTESIAN_POINT('Ctrl Pts',(-207.710038713311,92.9223390871439,9.00267799087017));
#20732=CARTESIAN_POINT('Ctrl Pts',(-204.721222346873,91.5965799970367,9.16158630967447));
#20733=CARTESIAN_POINT('Ctrl Pts',(-201.987986216981,93.3910383263244,9.32049462847878));
#20734=CARTESIAN_POINT('Ctrl Pts',(-202.016130658706,96.660574735006,9.47940294728309));
#20735=CARTESIAN_POINT('Ctrl Pts',(-204.779853162439,98.4077147865346,9.63831126608739));
#20736=CARTESIAN_POINT('Ctrl Pts',(-207.745403826312,97.0307000090919,9.7972195848917));
#20737=CARTESIAN_POINT('Ctrl Pts',(-208.193998947033,93.7919621600278,9.956127903696));
#20738=CARTESIAN_POINT('Ctrl Pts',(-205.71437153178,91.6607399006612,10.1150362225003));
#20739=CARTESIAN_POINT('Ctrl Pts',(-202.579816280574,92.5909139781486,10.2739445413046));
#20740=CARTESIAN_POINT('Ctrl Pts',(-201.664058413444,95.7297111946129,10.4328528601089));
#20741=CARTESIAN_POINT('Ctrl Pts',(-203.80665450774,98.1995173436874,10.5917611789132));
#20742=CARTESIAN_POINT('Ctrl Pts',(-207.043296411563,97.736041752413,10.7506694977175));
#20743=CARTESIAN_POINT('Ctrl Pts',(-208.406667002767,94.7641936626994,10.9095778165219));
#20744=CARTESIAN_POINT('Ctrl Pts',(-206.646843361447,92.0085301874643,11.0684861353262));
#20745=CARTESIAN_POINT('Ctrl Pts',(-203.37721213278,91.9954128013223,11.2273944541305));
#20746=CARTESIAN_POINT('Ctrl Pts',(-201.595334683216,94.7368673772781,11.3863027729348));
#20747=CARTESIAN_POINT('Ctrl Pts',(-202.934816342839,97.7195590007664,11.5452110917391));
#20748=CARTESIAN_POINT('Ctrl Pts',(-206.167635297217,98.2089893283008,11.7041194105434));
#20749=CARTESIAN_POINT('Ctrl Pts',(-208.329979261524,95.7564541058591,11.8630277293477));
#20750=CARTESIAN_POINT('Ctrl Pts',(-207.439435457357,92.6104102138975,12.021936048152));
#20751=CARTESIAN_POINT('Ctrl Pts',(-204.312444490949,91.6551155298822,12.1808443669563));
#20752=CARTESIAN_POINT('Ctrl Pts',(-201.815796730576,93.7663735429921,12.3397526857606));
#20753=CARTESIAN_POINT('Ctrl Pts',(-202.238390938423,97.0086065038919,12.4986610045649));
#20754=CARTESIAN_POINT('Ctrl Pts',(-205.192797468005,98.4093714718177,12.6575693233692));
#20755=CARTESIAN_POINT('Ctrl Pts',(-207.970449433746,96.6844627801914,12.8164776421735));
#20756=CARTESIAN_POINT('Ctrl Pts',(-208.024826558792,93.4152574386389,12.9753859609778));
#20757=CARTESIAN_POINT('Ctrl Pts',(-205.306076502467,91.5989263648761,13.1342942797821));
#20758=CARTESIAN_POINT('Ctrl Pts',(-202.306718929906,92.9006615869591,13.2932025985864));
#20759=CARTESIAN_POINT('Ctrl Pts',(-201.776531339599,96.1270468017065,13.4521109173908));
#20760=CARTESIAN_POINT('Ctrl Pts',(-204.201583790268,98.3201681065354,13.6110192361951));
#20761=CARTESIAN_POINT('Ctrl Pts',(-207.358615295882,97.4693963978157,13.7699275549994));
#20762=CARTESIAN_POINT('Ctrl Pts',(-208.353294664959,94.3547096762863,13.9288358738037));
#20763=CARTESIAN_POINT('Ctrl Pts',(-206.273710954002,91.8316179013893,14.087744192608));
#20764=CARTESIAN_POINT('Ctrl Pts',(-203.026403297675,92.2132634425565,14.2466525114123));
#20765=CARTESIAN_POINT('Ctrl Pts',(-201.588466995615,95.149757870614,14.4055608302166));
#20766=CARTESIAN_POINT('Ctrl Pts',(-203.278186112823,97.9489560439418,14.5644691490209));
#20767=CARTESIAN_POINT('Ctrl Pts',(-206.546444769616,98.0445840957001,14.7233774678252));
#20768=CARTESIAN_POINT('Ctrl Pts',(-208.396940534228,95.3489718500814,14.8822857866295));
#20769=CARTESIAN_POINT('Ctrl Pts',(-207.133158381155,92.333425341801,15.0411941054338));
#20770=CARTESIAN_POINT('Ctrl Pts',(-203.913722125861,91.7625662701771,15.2001024242381));
#20771=CARTESIAN_POINT('Ctrl Pts',(-201.690169853043,94.1597469629018,15.3590107430424));
#20772=CARTESIAN_POINT('Ctrl Pts',(-202.501039959935,97.3272690609605,15.5179190618467));
#20773=CARTESIAN_POINT('Ctrl Pts',(-205.602914034251,98.3611628114263,15.676827380651));
#20774=CARTESIAN_POINT('Ctrl Pts',(-208.152073583596,96.3136091809913,15.8357356994554));
#20775=CARTESIAN_POINT('Ctrl Pts',(-207.81138461072,93.0616931366079,15.9946440182597));
#20776=CARTESIAN_POINT('Ctrl Pts',(-204.893379258318,91.5869196180898,16.153552337064));
#20777=CARTESIAN_POINT('Ctrl Pts',(-202.072854649901,93.240962742727,16.3124606558683));
#20778=CARTESIAN_POINT('Ctrl Pts',(-201.936458165303,96.5082036173204,16.4713689746726));
#20779=CARTESIAN_POINT('Ctrl Pts',(-204.607536991561,98.3916410110266,16.6302772934769));
#20780=CARTESIAN_POINT('Ctrl Pts',(-207.640789093081,97.1679526977402,16.7891856122812));
#20781=CARTESIAN_POINT('Ctrl Pts',(-208.248035655587,93.9520682487087,16.9480939310855));
#20782=CARTESIAN_POINT('Ctrl Pts',(-206.674550837501,92.4580814192126,17.0540328102884));
#20783=CARTESIAN_POINT('Ctrl Pts',(-205.745932854347,92.2098224301579,17.1070022498898));
#20784=CARTESIAN_POINT('Ctrl Pts',(-207.336062657696,96.9973015569306,-0.321006749669432));
#20785=CARTESIAN_POINT('Ctrl Pts',(-208.000798179763,96.2198206477731,-0.268037310067996));
#20786=CARTESIAN_POINT('Ctrl Pts',(-208.480159627562,93.9611364831289,-0.162098430865125));
#20787=CARTESIAN_POINT('Ctrl Pts',(-206.009110847521,91.5068978920026,-0.00319011206081825));
#20788=CARTESIAN_POINT('Ctrl Pts',(-202.611368765802,92.2621562547108,0.155718206743488));
#20789=CARTESIAN_POINT('Ctrl Pts',(-201.404191313785,95.5240012055474,0.314626525547795));
#20790=CARTESIAN_POINT('Ctrl Pts',(-203.493269023741,98.307102300781,0.473534844352101));
#20791=CARTESIAN_POINT('Ctrl Pts',(-206.963865970602,98.0574884319591,0.632443163156409));
#20792=CARTESIAN_POINT('Ctrl Pts',(-208.633932648393,95.0051905167663,0.791351481960714));
#20793=CARTESIAN_POINT('Ctrl Pts',(-206.972489133437,91.9479467192658,0.950259800765022));
#20794=CARTESIAN_POINT('Ctrl Pts',(-203.50267093535,91.6888818401662,1.10916811956933));
#20795=CARTESIAN_POINT('Ctrl Pts',(-201.405596329389,94.4653692682509,1.26807643837364));
#20796=CARTESIAN_POINT('Ctrl Pts',(-202.603826461693,97.7320213682048,1.42698475717794));
#20797=CARTESIAN_POINT('Ctrl Pts',(-205.998843827582,98.4939765624303,1.58589307598225));
#20798=CARTESIAN_POINT('Ctrl Pts',(-208.478131313111,96.0526980537919,1.74480139478655));
#20799=CARTESIAN_POINT('Ctrl Pts',(-207.768707380001,92.6463153370295,1.90370971359086));
#20800=CARTESIAN_POINT('Ctrl Pts',(-204.520963226813,91.3977655726169,2.06261803239517));
#20801=CARTESIAN_POINT('Ctrl Pts',(-201.712394748966,93.4517035087255,2.22152635119947));
#20802=CARTESIAN_POINT('Ctrl Pts',(-201.917865964382,96.9251026344312,2.38043467000378));
#20803=CARTESIAN_POINT('Ctrl Pts',(-204.949003242364,98.6335890500974,2.53934298880809));
#20804=CARTESIAN_POINT('Ctrl Pts',(-208.026893764665,97.0108417000006,2.69825130761239));
#20805=CARTESIAN_POINT('Ctrl Pts',(-208.329761920824,93.5445771233942,2.8571596264167));
#20806=CARTESIAN_POINT('Ctrl Pts',(-205.579941560967,91.4126279879542,3.01606794522101));
#20807=CARTESIAN_POINT('Ctrl Pts',(-202.298437261384,92.5695414106573,3.17497626402532));
#20808=CARTESIAN_POINT('Ctrl Pts',(-201.49369548504,95.9546721068121,3.33388458282962));
#20809=CARTESIAN_POINT('Ctrl Pts',(-203.903494499117,98.4645700839332,3.49279290163393));
#20810=CARTESIAN_POINT('Ctrl Pts',(-207.318557500821,97.7981889317011,3.65170122043824));
#20811=CARTESIAN_POINT('Ctrl Pts',(-208.607992899891,94.5664594412711,3.81060953924254));
#20812=CARTESIAN_POINT('Ctrl Pts',(-206.589660734093,91.732195089681,3.96951785804685));
#20813=CARTESIAN_POINT('Ctrl Pts',(-203.113945374607,91.8938177561992,4.12842617685116));
#20814=CARTESIAN_POINT('Ctrl Pts',(-201.367343815629,94.903153586722,4.28733449565546));
#20815=CARTESIAN_POINT('Ctrl Pts',(-202.95112084504,98.0012771264839,4.44624281445977));
#20816=CARTESIAN_POINT('Ctrl Pts',(-206.413287383817,98.3478633413499,4.60515113326407));
#20817=CARTESIAN_POINT('Ctrl Pts',(-208.579767845133,95.6251658632375,4.76405945206838));
#20818=CARTESIAN_POINT('Ctrl Pts',(-207.464357156355,92.3293233090611,4.92296777087269));
#20819=CARTESIAN_POINT('Ctrl Pts',(-204.089651370241,91.481927295535,5.081876089677));
#20820=CARTESIAN_POINT('Ctrl Pts',(-201.549543033112,93.8598610166918,5.2407844084813));
#20821=CARTESIAN_POINT('Ctrl Pts',(-202.172775078182,97.2830614146476,5.3996927272856));
#20822=CARTESIAN_POINT('Ctrl Pts',(-205.387975332266,98.61317662496,5.55860104608992));
#20823=CARTESIAN_POINT('Ctrl Pts',(-208.247484138049,96.6307718892372,5.71750936489422));
#20824=CARTESIAN_POINT('Ctrl Pts',(-208.129735782527,93.1532937122619,5.87641768369853));
#20825=CARTESIAN_POINT('Ctrl Pts',(-205.142680641995,91.3688552196306,6.03532600250283));
#20826=CARTESIAN_POINT('Ctrl Pts',(-202.024817483593,92.9134096770875,6.19423432130715));
#20827=CARTESIAN_POINT('Ctrl Pts',(-201.634568403234,96.3709268212019,6.35314264011144));
#20828=CARTESIAN_POINT('Ctrl Pts',(-204.329709396056,98.5715935782041,6.51205095891576));
#20829=CARTESIAN_POINT('Ctrl Pts',(-207.639365322875,97.4978632616717,6.67095927772006));
#20830=CARTESIAN_POINT('Ctrl Pts',(-208.529280621322,94.13411982494,6.82986759652437));
#20831=CARTESIAN_POINT('Ctrl Pts',(-206.183590892181,91.5642056549396,6.98877591532867));
#20832=CARTESIAN_POINT('Ctrl Pts',(-202.752798261839,92.1441893393276,7.14768423413298));
#20833=CARTESIAN_POINT('Ctrl Pts',(-201.382215068533,95.3423483186146,7.30659255293729));
#20834=CARTESIAN_POINT('Ctrl Pts',(-203.328376665162,98.2266461857523,7.46550087174159));
#20835=CARTESIAN_POINT('Ctrl Pts',(-206.807063851782,98.1527908933495,7.6244091905459));
#20836=CARTESIAN_POINT('Ctrl Pts',(-208.629055096267,95.1884921480159,7.78331750935021));
#20837=CARTESIAN_POINT('Ctrl Pts',(-207.123969189693,92.0513859081191,7.94222582815452));
#20838=CARTESIAN_POINT('Ctrl Pts',(-203.671652069173,91.6175361116086,8.10113414695882));
#20839=CARTESIAN_POINT('Ctrl Pts',(-201.437149484965,94.2846914028758,8.26004246576313));
#20840=CARTESIAN_POINT('Ctrl Pts',(-202.469028431698,97.6076336211302,8.41895078456744));
#20841=CARTESIAN_POINT('Ctrl Pts',(-205.821273824104,98.5399264805142,8.57785910337175));
#20842=CARTESIAN_POINT('Ctrl Pts',(-208.420584553779,96.2268543075893,8.73676742217604));
#20843=CARTESIAN_POINT('Ctrl Pts',(-207.883941595716,92.7890158177634,8.89567574098036));
#20844=CARTESIAN_POINT('Ctrl Pts',(-204.70333321592,91.3781829144989,9.05458405978466));
#20845=CARTESIAN_POINT('Ctrl Pts',(-201.794705627984,93.2877914349212,9.21349237858898));
#20846=CARTESIAN_POINT('Ctrl Pts',(-201.824656095401,96.7671336308065,9.37240069739327));
#20847=CARTESIAN_POINT('Ctrl Pts',(-204.765726364391,98.6263874648557,9.53130901619759));
#20848=CARTESIAN_POINT('Ctrl Pts',(-207.92157608408,97.1610098025081,9.69021733500189));
#20849=CARTESIAN_POINT('Ctrl Pts',(-208.398957503736,93.7144425063808,9.84912565380619));
#20850=CARTESIAN_POINT('Ctrl Pts',(-205.760212673412,91.4464599519933,10.0080339726105));
#20851=CARTESIAN_POINT('Ctrl Pts',(-202.424513360844,92.4363231964359,10.1669422914148));
#20852=CARTESIAN_POINT('Ctrl Pts',(-201.449991413372,95.7765366807004,10.3258506102191));
#20853=CARTESIAN_POINT('Ctrl Pts',(-203.730077660409,98.4048300152887,10.4847589290234));
#20854=CARTESIAN_POINT('Ctrl Pts',(-207.174414514723,97.9116132469416,10.6436672478277));
#20855=CARTESIAN_POINT('Ctrl Pts',(-208.625272444921,94.7490619962975,10.802575566632));
#20856=CARTESIAN_POINT('Ctrl Pts',(-206.752521116536,91.8165679027658,10.9614838854363));
#20857=CARTESIAN_POINT('Ctrl Pts',(-203.273078016077,91.802608775416,11.1203922042406));
#20858=CARTESIAN_POINT('Ctrl Pts',(-201.376857689029,94.7199821861842,11.279300523045));
#20859=CARTESIAN_POINT('Ctrl Pts',(-202.802293737567,97.8940727989574,11.4382088418493));
#20860=CARTESIAN_POINT('Ctrl Pts',(-206.242562324195,98.4149098161,11.5971171606536));
#20861=CARTESIAN_POINT('Ctrl Pts',(-208.543663659863,95.8049956815827,11.7560254794579));
#20862=CARTESIAN_POINT('Ctrl Pts',(-207.595973758966,92.4570705034615,11.9149337982622));
#20863=CARTESIAN_POINT('Ctrl Pts',(-204.268324130509,91.4404746659679,12.0738421170665));
#20864=CARTESIAN_POINT('Ctrl Pts',(-201.611466761415,93.6872118706398,12.2327504358708));
#20865=CARTESIAN_POINT('Ctrl Pts',(-202.061178792513,97.1374985595401,12.3916587546751));
#20866=CARTESIAN_POINT('Ctrl Pts',(-205.205169260054,98.628150459449,12.5505670734794));
#20867=CARTESIAN_POINT('Ctrl Pts',(-208.161062843079,96.7925545691908,12.7094753922837));
#20868=CARTESIAN_POINT('Ctrl Pts',(-208.218929342183,93.3135646849756,12.868383711088));
#20869=CARTESIAN_POINT('Ctrl Pts',(-205.325717397541,91.3806798485012,13.0272920298923));
#20870=CARTESIAN_POINT('Ctrl Pts',(-202.133891383599,92.765947274806,13.1862003486966));
#20871=CARTESIAN_POINT('Ctrl Pts',(-201.569681714672,96.1993692694483,13.3451086675009));
#20872=CARTESIAN_POINT('Ctrl Pts',(-204.150349511013,98.5332229241514,13.5040169863052));
#20873=CARTESIAN_POINT('Ctrl Pts',(-207.50996737673,97.6278572896369,13.6629253051096));
#20874=CARTESIAN_POINT('Ctrl Pts',(-208.568475210139,94.3133014680822,13.8218336239139));
#20875=CARTESIAN_POINT('Ctrl Pts',(-206.355444844063,91.6283031749969,13.9807419427182));
#20876=CARTESIAN_POINT('Ctrl Pts',(-202.899757817094,92.0344388680353,14.1396502615225));
#20877=CARTESIAN_POINT('Ctrl Pts',(-201.369549302679,95.1593678164922,14.2985585803268));
#20878=CARTESIAN_POINT('Ctrl Pts',(-203.167697507449,98.1381902248446,14.4574668991311));
#20879=CARTESIAN_POINT('Ctrl Pts',(-206.645679958249,98.2399547180336,14.6163752179354));
#20880=CARTESIAN_POINT('Ctrl Pts',(-208.614921829979,95.3713653348348,14.7752835367397));
#20881=CARTESIAN_POINT('Ctrl Pts',(-207.270042916896,92.1623115429714,14.934191855544));
#20882=CARTESIAN_POINT('Ctrl Pts',(-203.844015795661,91.5548205083004,15.0931001743483));
#20883=CARTESIAN_POINT('Ctrl Pts',(-201.477778421142,94.1058280190935,15.2520084931526));
#20884=CARTESIAN_POINT('Ctrl Pts',(-202.340681972483,97.4766096574051,15.4109168119569));
#20885=CARTESIAN_POINT('Ctrl Pts',(-205.64160296068,98.5768482546894,15.5698251307612));
#20886=CARTESIAN_POINT('Ctrl Pts',(-208.354341794396,96.3979033358336,15.7287334495655));
#20887=CARTESIAN_POINT('Ctrl Pts',(-207.991790848075,92.937312201061,15.8876417683699));
#20888=CARTESIAN_POINT('Ctrl Pts',(-204.886537417199,91.367902630111,16.0465500871741));
#20889=CARTESIAN_POINT('Ctrl Pts',(-201.885020058793,93.1280855178388,16.2054584059785));
#20890=CARTESIAN_POINT('Ctrl Pts',(-201.739871026969,96.6049848754692,16.3643667247828));
#20891=CARTESIAN_POINT('Ctrl Pts',(-204.582352684019,98.6092822369636,16.5232750435871));
#20892=CARTESIAN_POINT('Ctrl Pts',(-207.810248235069,97.3070699809007,16.6821833623914));
#20893=CARTESIAN_POINT('Ctrl Pts',(-208.45646174186,93.8848225849406,16.8410916811957));
#20894=CARTESIAN_POINT('Ctrl Pts',(-206.782006578242,92.2949667869871,16.9470305603986));
#20895=CARTESIAN_POINT('Ctrl Pts',(-205.793799282533,92.0307770462543,17.));
#20896=CARTESIAN_POINT('Ctrl Pts',(-206.913465996665,96.6359872033749,0.));
#20897=CARTESIAN_POINT('Ctrl Pts',(-206.975062233787,96.5781018655823,3.0968450357692E-17));
#20898=CARTESIAN_POINT('Ctrl Pts',(-207.033286127394,96.517064861521,4.93396470770506E-17));
#20899=CARTESIAN_POINT('Ctrl Pts',(-207.088141455004,96.4532612528611,2.77555756156289E-17));
#20900=CARTESIAN_POINT('Ctrl Pts',(-207.144450798064,96.3877664423286,5.59938883280038E-18));
#20901=CARTESIAN_POINT('Ctrl Pts',(-207.197211066199,96.3193559864889,1.56478474477103E-16));
#20902=CARTESIAN_POINT('Ctrl Pts',(-207.246400774978,96.2483978328537,8.32667268468867E-17));
#20903=CARTESIAN_POINT('Ctrl Pts',(-207.297350807049,96.1749003413407,7.43499329068896E-18));
#20904=CARTESIAN_POINT('Ctrl Pts',(-207.344470743098,96.0986690282088,2.71682604868357E-17));
#20905=CARTESIAN_POINT('Ctrl Pts',(-207.387701617095,96.0200685851594,-3.46944695195361E-17));
#20906=CARTESIAN_POINT('Ctrl Pts',(-207.406615124468,95.9856808913252,-6.17594138973238E-17));
#20907=CARTESIAN_POINT('Ctrl Pts',(-207.424783744567,95.9508392224169,2.01136707471298E-16));
#20908=CARTESIAN_POINT('Ctrl Pts',(-207.442200082494,95.9155720190512,2.15105711021124E-16));
#20909=CARTESIAN_POINT('Ctrl Pts',(-207.451657198057,95.8964218383858,2.22690915294919E-16));
#20910=CARTESIAN_POINT('Ctrl Pts',(-207.460892474714,95.8771461685267,3.72933574804102E-16));
#20911=CARTESIAN_POINT('Ctrl Pts',(-207.469904527905,95.8577494362717,3.88578058618805E-16));
#20912=CARTESIAN_POINT('Ctrl Pts',(-207.478555310542,95.8391302702473,4.03595394409402E-16));
#20913=CARTESIAN_POINT('Ctrl Pts',(-207.487002900789,95.8203935450865,3.88581800676704E-16));
#20914=CARTESIAN_POINT('Ctrl Pts',(-207.495231967652,95.8015759912223,3.60822483003176E-16));
#20915=CARTESIAN_POINT('Ctrl Pts',(-207.531772133063,95.7180189437175,2.37560626425314E-16));
#20916=CARTESIAN_POINT('Ctrl Pts',(-207.564052932394,95.6327781953704,1.86682596890399E-16));
#20917=CARTESIAN_POINT('Ctrl Pts',(-207.592050831023,95.5462530210923,2.22044604925031E-16));
#20918=CARTESIAN_POINT('Ctrl Pts',(-207.620513276378,95.458292203845,2.57993346458143E-16));
#20919=CARTESIAN_POINT('Ctrl Pts',(-207.644550007454,95.3690032283074,-2.49369539605486E-16));
#20920=CARTESIAN_POINT('Ctrl Pts',(-207.664097180383,95.278768433218,-3.46944695195361E-16));
#20921=CARTESIAN_POINT('Ctrl Pts',(-207.683347083547,95.1899059120856,-4.43035945993059E-16));
#20922=CARTESIAN_POINT('Ctrl Pts',(-207.698243217594,95.1001252116962,-1.09324133867228E-16));
#20923=CARTESIAN_POINT('Ctrl Pts',(-207.708681596094,95.0097684816411,-1.94289029309402E-16));
#20924=CARTESIAN_POINT('Ctrl Pts',(-207.712775443857,94.9743313017009,-2.27611575250926E-16));
#20925=CARTESIAN_POINT('Ctrl Pts',(-207.716183130269,94.9388053405125,4.4208590596913E-16));
#20926=CARTESIAN_POINT('Ctrl Pts',(-207.71889639163,94.903210714114,4.85722573273506E-16));
#20927=CARTESIAN_POINT('Ctrl Pts',(-207.720491854529,94.8822802182006,5.1138198254676E-16));
#20928=CARTESIAN_POINT('Ctrl Pts',(-207.721847182612,94.8613259758214,7.42875535366934E-17));
#20929=CARTESIAN_POINT('Ctrl Pts',(-207.722960502641,94.8403520552435,6.93889390390723E-17));
#20930=CARTESIAN_POINT('Ctrl Pts',(-207.723721970302,94.8260067081621,6.60384769771266E-17));
#20931=CARTESIAN_POINT('Ctrl Pts',(-207.724370161868,94.8116517728123,2.77396210343816E-16));
#20932=CARTESIAN_POINT('Ctrl Pts',(-207.724904092468,94.7973039113478,2.77555756156289E-16));
#20933=CARTESIAN_POINT('Ctrl Pts',(-207.728446434094,94.7021135872458,2.78614256591085E-16));
#20934=CARTESIAN_POINT('Ctrl Pts',(-207.726972757336,94.6070734840445,4.25745817027648E-17));
#20935=CARTESIAN_POINT('Ctrl Pts',(-207.720425227949,94.5125829664624,2.77555756156289E-17));
#20936=CARTESIAN_POINT('Ctrl Pts',(-207.713899630728,94.41840896242,1.29862085419292E-17));
#20937=CARTESIAN_POINT('Ctrl Pts',(-207.702334474037,94.3247799136568,-6.21676310273157E-17));
#20938=CARTESIAN_POINT('Ctrl Pts',(-207.685624510351,94.2320732634053,-8.32667268468867E-17));
#20939=CARTESIAN_POINT('Ctrl Pts',(-207.683541691529,94.2205178130349,-8.58966304615819E-17));
#20940=CARTESIAN_POINT('Ctrl Pts',(-207.681378875184,94.2089766813724,8.3661212389091E-17));
#20941=CARTESIAN_POINT('Ctrl Pts',(-207.679135800651,94.197450591266,8.32667268468867E-17));
#20942=CARTESIAN_POINT('Ctrl Pts',(-207.661515002607,94.1069057150043,8.1200767834121E-17));
#20943=CARTESIAN_POINT('Ctrl Pts',(-207.638945751039,94.017288753037,1.06755513380276E-16));
#20944=CARTESIAN_POINT('Ctrl Pts',(-207.611703055832,93.9288370382536,1.38777878078145E-16));
#20945=CARTESIAN_POINT('Ctrl Pts',(-207.600776295581,93.8933599801309,1.51621713795702E-16));
#20946=CARTESIAN_POINT('Ctrl Pts',(-207.589097112068,93.8580704314563,2.10854356106776E-16));
#20947=CARTESIAN_POINT('Ctrl Pts',(-207.576680955897,93.8229840703899,2.4980018054066E-16));
#20948=CARTESIAN_POINT('Ctrl Pts',(-207.570899597757,93.8066467421239,2.67934597990291E-16));
#20949=CARTESIAN_POINT('Ctrl Pts',(-207.564958436528,93.7903534718742,8.50030008580217E-17));
#20950=CARTESIAN_POINT('Ctrl Pts',(-207.55885894084,93.7741058681104,8.32667268468867E-17));
#20951=CARTESIAN_POINT('Ctrl Pts',(-207.553795395264,93.7606177887079,8.18253449626879E-17));
#20952=CARTESIAN_POINT('Ctrl Pts',(-207.54862605565,93.7471700690316,4.26988678161571E-17));
#20953=CARTESIAN_POINT('Ctrl Pts',(-207.543352966221,93.7337654693977,5.55111512312578E-17));
#20954=CARTESIAN_POINT('Ctrl Pts',(-207.509119317179,93.646740895753,1.38690323460505E-16));
#20955=CARTESIAN_POINT('Ctrl Pts',(-207.470507251376,93.5615075862816,3.77458317449025E-16));
#20956=CARTESIAN_POINT('Ctrl Pts',(-207.427849249462,93.4782966850494,3.60822483003176E-16));
#20957=CARTESIAN_POINT('Ctrl Pts',(-207.383612733185,93.3920066521892,3.43571057051397E-16));
#20958=CARTESIAN_POINT('Ctrl Pts',(-207.335025179508,93.3078907458115,-1.10988550360456E-16));
#20959=CARTESIAN_POINT('Ctrl Pts',(-207.282401401832,93.2262103191478,-2.22044604925031E-16));
#20960=CARTESIAN_POINT('Ctrl Pts',(-207.22920174438,93.1436360359813,-3.34315983412545E-16));
#20961=CARTESIAN_POINT('Ctrl Pts',(-207.171876621466,93.0635500123343,3.41627951812914E-16));
#20962=CARTESIAN_POINT('Ctrl Pts',(-207.11069968939,92.9862376762064,4.44089209850063E-16));
#20963=CARTESIAN_POINT('Ctrl Pts',(-207.086606803213,92.955790295941,4.8444081532694E-16));
#20964=CARTESIAN_POINT('Ctrl Pts',(-207.061915990083,92.9257733393162,2.50658725338041E-16));
#20965=CARTESIAN_POINT('Ctrl Pts',(-207.036642028582,92.896205321917,2.4980018054066E-16));
#20966=CARTESIAN_POINT('Ctrl Pts',(-207.022295011884,92.8794207414964,2.49312819010743E-16));
#20967=CARTESIAN_POINT('Ctrl Pts',(-207.007760063825,92.8627808390425,4.63072277927187E-16));
#20968=CARTESIAN_POINT('Ctrl Pts',(-206.993039745212,92.8462891116921,4.71844785465692E-16));
#20969=CARTESIAN_POINT('Ctrl Pts',(-206.979027736376,92.8305909304621,4.80195178984602E-16));
#20970=CARTESIAN_POINT('Ctrl Pts',(-206.964844946112,92.8150241309821,9.01246990176946E-16));
#20971=CARTESIAN_POINT('Ctrl Pts',(-206.950512567364,92.7996118404543,8.60422844084496E-16));
#20972=CARTESIAN_POINT('Ctrl Pts',(-206.881794961135,92.7257165206168,6.64688580759402E-16));
#20973=CARTESIAN_POINT('Ctrl Pts',(-206.809566114702,92.655283034501,1.95353569017064E-16));
#20974=CARTESIAN_POINT('Ctrl Pts',(-206.734139541689,92.5885980814127,2.22044604925031E-16));
#20975=CARTESIAN_POINT('Ctrl Pts',(-206.669026438941,92.5310313111255,2.45086035737897E-16));
#20976=CARTESIAN_POINT('Ctrl Pts',(-206.601529266805,92.4762579626061,-8.3008266997134E-17));
#20977=CARTESIAN_POINT('Ctrl Pts',(-206.531823161522,92.42447802842,-1.66533453693773E-16));
#20978=CARTESIAN_POINT('Ctrl Pts',(-206.504658151372,92.4042989862542,-1.99083867106794E-16));
#20979=CARTESIAN_POINT('Ctrl Pts',(-206.477157425522,92.384574749707,2.57352051279242E-16));
#20980=CARTESIAN_POINT('Ctrl Pts',(-206.449330482091,92.3653179595526,2.77555756156289E-16));
#20981=CARTESIAN_POINT('Ctrl Pts',(-206.434060293588,92.3547506898726,2.88642650506663E-16));
#20982=CARTESIAN_POINT('Ctrl Pts',(-206.4186931394,92.344325166916,5.01730169144111E-17));
#20983=CARTESIAN_POINT('Ctrl Pts',(-206.403240754609,92.3340499669156,5.55111512312578E-17));
#20984=CARTESIAN_POINT('Ctrl Pts',(-206.316661516034,92.2764783361116,8.54205542659342E-17));
#20985=CARTESIAN_POINT('Ctrl Pts',(-206.227325727871,92.2235642261423,1.65945870128525E-16));
#20986=CARTESIAN_POINT('Ctrl Pts',(-206.135543256089,92.1756305450252,5.55111512312578E-17));
#20987=CARTESIAN_POINT('Ctrl Pts',(-206.043760784307,92.1276968639081,-5.49235676660085E-17));
#20988=CARTESIAN_POINT('Ctrl Pts',(-205.949530976973,92.0847426931351,-5.98436115446713E-17));
#20989=CARTESIAN_POINT('Ctrl Pts',(-205.853125481029,92.0471321793771,-2.22044604925031E-16));
#20990=CARTESIAN_POINT('Ctrl Pts',(-205.834025098342,92.03968057925,-2.54180750436268E-16));
#20991=CARTESIAN_POINT('Ctrl Pts',(-205.814839209604,92.0324388923413,-1.04868572471002E-16));
#20992=CARTESIAN_POINT('Ctrl Pts',(-205.79557093555,92.025406175614,-1.11022302462516E-16));
#20993=CARTESIAN_POINT('Ctrl Pts',(-202.480282650156,94.9980775783256,1.61258330249198));
#20994=CARTESIAN_POINT('Ctrl Pts',(-202.479237247099,94.8744698806693,1.60474993100901));
#20995=CARTESIAN_POINT('Ctrl Pts',(-202.487545284979,94.7510033134378,1.59691655952604));
#20996=CARTESIAN_POINT('Ctrl Pts',(-202.505691786454,94.6290001821137,1.58908318804307));
#20997=CARTESIAN_POINT('Ctrl Pts',(-202.628398850194,93.8040121791943,1.53611374844163));
#20998=CARTESIAN_POINT('Ctrl Pts',(-203.200969244479,93.0459397210627,1.4831443088402));
#20999=CARTESIAN_POINT('Ctrl Pts',(-203.960941731557,92.702270111656,1.43017486923876));
#21000=CARTESIAN_POINT('Ctrl Pts',(-204.720914218634,92.3586005022492,1.37720542963732));
#21001=CARTESIAN_POINT('Ctrl Pts',(-205.668288798503,92.4293337415673,1.32423599003589));
#21002=CARTESIAN_POINT('Ctrl Pts',(-206.368790472088,92.8820644553757,1.27126655043445));
#21003=CARTESIAN_POINT('Ctrl Pts',(-207.069292145673,93.3347951691841,1.21829711083302));
#21004=CARTESIAN_POINT('Ctrl Pts',(-207.522920912975,94.1695233574828,1.16532767123158));
#21005=CARTESIAN_POINT('Ctrl Pts',(-207.521743709329,95.0035763514476,1.11235823163015));
#21006=CARTESIAN_POINT('Ctrl Pts',(-207.520566505683,95.8376293454124,1.05938879202871));
#21007=CARTESIAN_POINT('Ctrl Pts',(-207.064583331089,96.6710071450434,1.00641935242728));
#21008=CARTESIAN_POINT('Ctrl Pts',(-206.362798141834,97.1217724460714,0.95344991282584));
#21009=CARTESIAN_POINT('Ctrl Pts',(-205.661012952578,97.5725377470994,0.900480473224404));
#21010=CARTESIAN_POINT('Ctrl Pts',(-204.713425748661,97.6406905495243,0.847511033622969));
#21011=CARTESIAN_POINT('Ctrl Pts',(-203.954438657476,97.2948278472581,0.794541594021534));
#21012=CARTESIAN_POINT('Ctrl Pts',(-203.195451566291,96.9489651449919,0.741572154420098));
#21013=CARTESIAN_POINT('Ctrl Pts',(-202.625064587839,96.1890869380346,0.688602714818662));
#21014=CARTESIAN_POINT('Ctrl Pts',(-202.504670688411,95.3638523156723,0.635633275217227));
#21015=CARTESIAN_POINT('Ctrl Pts',(-202.487207310037,95.2441503662684,0.627949950975477));
#21016=CARTESIAN_POINT('Ctrl Pts',(-202.479211825944,95.1230733120894,0.620266626733727));
#21017=CARTESIAN_POINT('Ctrl Pts',(-202.480223566112,95.0018649480296,0.612583302491977));
#21018=CARTESIAN_POINT('Ctrl Pts',(-204.206200717467,92.0307770462543,-1.66533453693773E-15));
#21019=CARTESIAN_POINT('Ctrl Pts',(-203.217993421758,92.294966786987,0.0529694396014339));
#21020=CARTESIAN_POINT('Ctrl Pts',(-201.543538204128,93.8848222016534,0.158908318804305));
#21021=CARTESIAN_POINT('Ctrl Pts',(-202.189751811533,97.3070700667118,0.317816637608612));
#21022=CARTESIAN_POINT('Ctrl Pts',(-205.417647311761,98.6092821234889,0.476724956412918));
#21023=CARTESIAN_POINT('Ctrl Pts',(-208.260128930045,96.6049848945777,0.635633275217225));
#21024=CARTESIAN_POINT('Ctrl Pts',(-208.114979909401,93.1280855192232,0.794541594021532));
#21025=CARTESIAN_POINT('Ctrl Pts',(-205.113462578231,91.3679026833885,0.953449912825839));
#21026=CARTESIAN_POINT('Ctrl Pts',(-202.008209188913,92.9373122193729,1.11235823163015));
#21027=CARTESIAN_POINT('Ctrl Pts',(-201.645658243496,96.3979033225417,1.27126655043445));
#21028=CARTESIAN_POINT('Ctrl Pts',(-204.35839704753,98.5768482113765,1.43017486923876));
#21029=CARTESIAN_POINT('Ctrl Pts',(-207.659317996079,97.4766096293226,1.58908318804307));
#21030=CARTESIAN_POINT('Ctrl Pts',(-208.522221537982,94.105828029106,1.74799150684737));
#21031=CARTESIAN_POINT('Ctrl Pts',(-206.155984190728,91.5548205487187,1.90689982565168));
#21032=CARTESIAN_POINT('Ctrl Pts',(-202.729957109659,92.1623115759729,2.06580814445599));
#21033=CARTESIAN_POINT('Ctrl Pts',(-201.385078212169,95.371365330558,2.22471646326029));
#21034=CARTESIAN_POINT('Ctrl Pts',(-203.354320060973,98.2399546801978,2.3836247820646));
#21035=CARTESIAN_POINT('Ctrl Pts',(-206.832302471161,98.13819018824,2.54253310086891));
#21036=CARTESIAN_POINT('Ctrl Pts',(-208.630450654962,95.1593678146252,2.70144141967321));
#21037=CARTESIAN_POINT('Ctrl Pts',(-207.100242158396,92.0344389026441,2.86034973847752));
#21038=CARTESIAN_POINT('Ctrl Pts',(-203.644555171756,91.6283032143389,3.01925805728183));
#21039=CARTESIAN_POINT('Ctrl Pts',(-201.4315248315,94.3133014760961,3.17816637608613));
#21040=CARTESIAN_POINT('Ctrl Pts',(-202.490032652559,97.6278572589721,3.33707469489044));
#21041=CARTESIAN_POINT('Ctrl Pts',(-205.849650479072,98.5332228829228,3.49598301369474));
#21042=CARTESIAN_POINT('Ctrl Pts',(-208.430318245301,96.1993692554529,3.65489133249905));
#21043=CARTESIAN_POINT('Ctrl Pts',(-207.866108582956,92.7659473008752,3.81379965130336));
#21044=CARTESIAN_POINT('Ctrl Pts',(-204.67428260626,91.3806798907347,3.97270797010767));
#21045=CARTESIAN_POINT('Ctrl Pts',(-201.781070695379,93.3135647046544,4.13161628891197));
#21046=CARTESIAN_POINT('Ctrl Pts',(-201.838937193807,96.7925545482736,4.29052460771628));
#21047=CARTESIAN_POINT('Ctrl Pts',(-204.79483074234,98.6281504171124,4.44943292652058));
#21048=CARTESIAN_POINT('Ctrl Pts',(-207.938821173194,97.1374985345979,4.60834124532489));
#21049=CARTESIAN_POINT('Ctrl Pts',(-208.388533199045,93.6872118859588,4.76724956412919));
#21050=CARTESIAN_POINT('Ctrl Pts',(-205.731675860954,91.4404747075036,4.92615788293351));
#21051=CARTESIAN_POINT('Ctrl Pts',(-202.404026271327,92.4570705331348,5.08506620173781));
#21052=CARTESIAN_POINT('Ctrl Pts',(-201.456336381487,95.8049956721891,5.24397452054212));
#21053=CARTESIAN_POINT('Ctrl Pts',(-203.757437690304,98.4149097762516,5.40288283934642));
#21054=CARTESIAN_POINT('Ctrl Pts',(-207.197706236788,97.8940727651868,5.56179115815073));
#21055=CARTESIAN_POINT('Ctrl Pts',(-208.623142268693,94.7199821894518,5.72069947695504));
#21056=CARTESIAN_POINT('Ctrl Pts',(-206.726921963772,91.8026088127262,5.87960779575934));
#21057=CARTESIAN_POINT('Ctrl Pts',(-203.247478903914,91.8165679399129,6.03851611456365));
#21058=CARTESIAN_POINT('Ctrl Pts',(-201.374727597382,94.7490619992257,6.19742443336796));
#21059=CARTESIAN_POINT('Ctrl Pts',(-202.82558551065,97.9116132129659,6.35633275217227));
#21060=CARTESIAN_POINT('Ctrl Pts',(-206.269922324772,98.4048299755582,6.51524107097657));
#21061=CARTESIAN_POINT('Ctrl Pts',(-208.550008545203,95.7765366716391,6.67414938978089));
#21062=CARTESIAN_POINT('Ctrl Pts',(-207.575486609103,92.4363232263514,6.83305770858518));
#21063=CARTESIAN_POINT('Ctrl Pts',(-204.239787335459,91.4464599934592,6.9919660273895));
#21064=CARTESIAN_POINT('Ctrl Pts',(-201.601042535926,93.7144425213819,7.1508743461938));
#21065=CARTESIAN_POINT('Ctrl Pts',(-202.078423950012,97.1610097772913,7.30978266499811));
#21066=CARTESIAN_POINT('Ctrl Pts',(-205.234273632875,98.6263874225397,7.46869098380241));
#21067=CARTESIAN_POINT('Ctrl Pts',(-208.175343867546,96.7671336101861,7.62759930260672));
#21068=CARTESIAN_POINT('Ctrl Pts',(-208.205294334613,93.2877914549009,7.78650762141103));
#21069=CARTESIAN_POINT('Ctrl Pts',(-205.296666780619,91.3781829567617,7.94541594021533));
#21070=CARTESIAN_POINT('Ctrl Pts',(-202.116058437936,92.789015843563,8.10432425901964));
#21071=CARTESIAN_POINT('Ctrl Pts',(-201.579415486135,96.2268542932731,8.26323257782395));
#21072=CARTESIAN_POINT('Ctrl Pts',(-204.17872618548,98.5399264392071,8.42214089662825));
#21073=CARTESIAN_POINT('Ctrl Pts',(-207.530971538769,97.6076335907019,8.58104921543256));
#21074=CARTESIAN_POINT('Ctrl Pts',(-208.56285047346,94.2846914112228,8.73995753423687));
#21075=CARTESIAN_POINT('Ctrl Pts',(-206.328347915327,91.6175361510784,8.89886585304118));
#21076=CARTESIAN_POINT('Ctrl Pts',(-202.876030835092,92.0513859425261,9.05777417184547));
#21077=CARTESIAN_POINT('Ctrl Pts',(-201.37094494608,95.1884921458163,9.2166824906498));
#21078=CARTESIAN_POINT('Ctrl Pts',(-203.192936169305,98.1527908565597,9.37559080945409));
#21079=CARTESIAN_POINT('Ctrl Pts',(-206.671623315332,98.2266461481009,9.5344991282584));
#21080=CARTESIAN_POINT('Ctrl Pts',(-208.617784889251,95.3423483146199,9.6934074470627));
#21081=CARTESIAN_POINT('Ctrl Pts',(-207.247201711938,92.1441893726518,9.85231576586701));
#21082=CARTESIAN_POINT('Ctrl Pts',(-203.81640912163,91.5642056950316,10.0112240846713));
#21083=CARTESIAN_POINT('Ctrl Pts',(-201.47071941986,94.1341198350438,10.1701324034756));
#21084=CARTESIAN_POINT('Ctrl Pts',(-202.360634707924,97.4978632325243,10.3290407222799));
#21085=CARTESIAN_POINT('Ctrl Pts',(-205.670290596122,98.5715935365275,10.4879490410842));
#21086=CARTESIAN_POINT('Ctrl Pts',(-208.365431557495,96.3709268052048,10.6468573598885));
#21087=CARTESIAN_POINT('Ctrl Pts',(-207.975182481689,92.9134097014358,10.8057656786928));
#21088=CARTESIAN_POINT('Ctrl Pts',(-204.85731935967,91.3688552620022,10.9646739974972));
#21089=CARTESIAN_POINT('Ctrl Pts',(-201.870264253993,93.153293733811,11.1235823163015));
#21090=CARTESIAN_POINT('Ctrl Pts',(-201.752515899846,96.6307718702076,11.2824906351058));
#21091=CARTESIAN_POINT('Ctrl Pts',(-204.612024672262,98.6131765827982,11.4413989539101));
#21092=CARTESIAN_POINT('Ctrl Pts',(-207.827224888828,97.2830613880067,11.6003072727144));
#21093=CARTESIAN_POINT('Ctrl Pts',(-208.450456926625,93.8598610299961,11.7592155915187));
#21094=CARTESIAN_POINT('Ctrl Pts',(-205.910348619136,91.4819273365871,11.918123910323));
#21095=CARTESIAN_POINT('Ctrl Pts',(-202.535642872402,92.3293233402249,12.0770322291273));
#21096=CARTESIAN_POINT('Ctrl Pts',(-201.420232196639,95.6251658559424,12.2359405479316));
#21097=CARTESIAN_POINT('Ctrl Pts',(-203.586712632674,98.3478633022839,12.3948488667359));
#21098=CARTESIAN_POINT('Ctrl Pts',(-207.048879131051,98.0012770914624,12.5537571855402));
#21099=CARTESIAN_POINT('Ctrl Pts',(-208.632656141981,94.9031535878521,12.7126655043445));
#21100=CARTESIAN_POINT('Ctrl Pts',(-206.886054603385,91.8938177924453,12.8715738231489));
#21101=CARTESIAN_POINT('Ctrl Pts',(-203.410339284457,91.7321951278126,13.0304821419532));
#21102=CARTESIAN_POINT('Ctrl Pts',(-201.39200714221,94.56645944633,13.1893904607574));
#21103=CARTESIAN_POINT('Ctrl Pts',(-202.681442526234,97.7981888990492,13.3482987795618));
#21104=CARTESIAN_POINT('Ctrl Pts',(-206.096505488088,98.4645700435054,13.5072070983661));
#21105=CARTESIAN_POINT('Ctrl Pts',(-208.506304474045,95.9546720956722,13.6661154171704));
#21106=CARTESIAN_POINT('Ctrl Pts',(-207.701562707091,92.569541439018,13.8250237359747));
#21107=CARTESIAN_POINT('Ctrl Pts',(-204.420058445801,91.4126280298156,13.983932054779));
#21108=CARTESIAN_POINT('Ctrl Pts',(-201.670238118031,93.5445771403762,14.1428403735833));
#21109=CARTESIAN_POINT('Ctrl Pts',(-201.973106270655,97.0108416765384,14.3017486923876));
#21110=CARTESIAN_POINT('Ctrl Pts',(-205.05099675704,98.6335890076928,14.4606570111919));
#21111=CARTESIAN_POINT('Ctrl Pts',(-208.082133999653,96.9251026119764,14.6195653299962));
#21112=CARTESIAN_POINT('Ctrl Pts',(-208.287605212672,93.451703526775,14.7784736488005));
#21113=CARTESIAN_POINT('Ctrl Pts',(-205.479036767596,91.3977656146854,14.9373819676048));
#21114=CARTESIAN_POINT('Ctrl Pts',(-202.231292652311,92.6463153644278,15.0962902864091));
#21115=CARTESIAN_POINT('Ctrl Pts',(-201.521868727466,96.0526980416367,15.2551986052134));
#21116=CARTESIAN_POINT('Ctrl Pts',(-204.001156184096,98.4939765214113,15.4141069240178));
#21117=CARTESIAN_POINT('Ctrl Pts',(-207.396173510293,97.7320213368001,15.573015242822));
#21118=CARTESIAN_POINT('Ctrl Pts',(-208.594403628795,94.4653692735856,15.7319235616264));
#21119=CARTESIAN_POINT('Ctrl Pts',(-206.497329046882,91.688881880511,15.8908318804307));
#21120=CARTESIAN_POINT('Ctrl Pts',(-203.027510890261,91.9479467516828,16.049740199235));
#21121=CARTESIAN_POINT('Ctrl Pts',(-201.366067392462,95.0051905226268,16.2086485180393));
#21122=CARTESIAN_POINT('Ctrl Pts',(-203.036134055811,98.0574883854641,16.3675568368436));
#21123=CARTESIAN_POINT('Ctrl Pts',(-206.506730950831,98.3071022816236,16.5264651556479));
#21124=CARTESIAN_POINT('Ctrl Pts',(-208.595808661615,95.5240011654517,16.6853734744522));
#21125=CARTESIAN_POINT('Ctrl Pts',(-207.388631166444,92.2621563458355,16.8442817932565));
#21126=CARTESIAN_POINT('Ctrl Pts',(-203.990889239491,91.5068978476827,17.0031901120608));
#21127=CARTESIAN_POINT('Ctrl Pts',(-201.519840110817,93.9611367684014,17.1620984308651));
#21128=CARTESIAN_POINT('Ctrl Pts',(-201.999201820237,96.219820647773,17.268037310068));
#21129=CARTESIAN_POINT('Ctrl Pts',(-202.663937342304,96.9973015569306,17.3210067496694));
#21130=CARTESIAN_POINT('Ctrl Pts',(-204.254067145653,92.2098224301578,-0.107002249889812));
#21131=CARTESIAN_POINT('Ctrl Pts',(-203.325449162499,92.4580814192125,-0.0540328102883767));
#21132=CARTESIAN_POINT('Ctrl Pts',(-201.751964293657,93.9520678885337,0.0519060689144946));
#21133=CARTESIAN_POINT('Ctrl Pts',(-202.359210950711,97.1679527783771,0.210814387718801));
#21134=CARTESIAN_POINT('Ctrl Pts',(-205.392463004474,98.3916409043943,0.369722706523108));
#21135=CARTESIAN_POINT('Ctrl Pts',(-208.063541794304,96.5082036352768,0.528631025327414));
#21136=CARTESIAN_POINT('Ctrl Pts',(-207.927145320211,93.2409627440279,0.687539344131721));
#21137=CARTESIAN_POINT('Ctrl Pts',(-205.106620737387,91.5869196681547,0.846447662936027));
#21138=CARTESIAN_POINT('Ctrl Pts',(-202.188615424038,93.0616931538156,1.00535598174034));
#21139=CARTESIAN_POINT('Ctrl Pts',(-201.847926452011,96.3136091685009,1.16426430054464));
#21140=CARTESIAN_POINT('Ctrl Pts',(-204.397085973464,98.3611627707252,1.32317261934895));
#21141=CARTESIAN_POINT('Ctrl Pts',(-207.498960010523,97.3272690345715,1.48208093815326));
#21142=CARTESIAN_POINT('Ctrl Pts',(-208.309830108546,94.1597469723104,1.64098925695756));
#21143=CARTESIAN_POINT('Ctrl Pts',(-206.086277861348,91.7625663081583,1.79989757576187));
#21144=CARTESIAN_POINT('Ctrl Pts',(-202.866841643798,92.3334253728125,1.95880589456617));
#21145=CARTESIAN_POINT('Ctrl Pts',(-201.603059505378,95.3489718460626,2.11771421337048));
#21146=CARTESIAN_POINT('Ctrl Pts',(-203.453555248447,98.0445840601458,2.27662253217479));
#21147=CARTESIAN_POINT('Ctrl Pts',(-206.721813867076,97.9489560095445,2.43553085097909));
#21148=CARTESIAN_POINT('Ctrl Pts',(-208.411532964581,95.1497578688597,2.5944391697834));
#21149=CARTESIAN_POINT('Ctrl Pts',(-206.973596679293,92.2132634750782,2.75334748858771));
#21150=CARTESIAN_POINT('Ctrl Pts',(-203.726289060862,91.8316179383591,2.91225580739202));
#21151=CARTESIAN_POINT('Ctrl Pts',(-201.64670537417,94.354709683817,3.07116412619632));
#21152=CARTESIAN_POINT('Ctrl Pts',(-202.641384731641,97.469396369,3.23007244500063));
#21153=CARTESIAN_POINT('Ctrl Pts',(-205.798416200415,98.3201680677929,3.38898076380494));
#21154=CARTESIAN_POINT('Ctrl Pts',(-208.223468622787,96.1270467885551,3.54788908260924));
#21155=CARTESIAN_POINT('Ctrl Pts',(-207.693281038666,92.9006616114564,3.70679740141355));
#21156=CARTESIAN_POINT('Ctrl Pts',(-204.693923501105,91.5989264045628,3.86570572021786));
#21157=CARTESIAN_POINT('Ctrl Pts',(-201.975173476504,93.4152574571311,4.02461403902216));
#21158=CARTESIAN_POINT('Ctrl Pts',(-202.029550600916,96.6844627605355,4.18352235782647));
#21159=CARTESIAN_POINT('Ctrl Pts',(-204.807202534245,98.4093714320339,4.34243067663077));
#21160=CARTESIAN_POINT('Ctrl Pts',(-207.761609029352,97.0086064804539,4.50133899543508));
#21161=CARTESIAN_POINT('Ctrl Pts',(-208.184203232267,93.7663735573872,4.66024731423939));
#21162=CARTESIAN_POINT('Ctrl Pts',(-205.687555501028,91.6551155689135,4.81915563304369));
#21163=CARTESIAN_POINT('Ctrl Pts',(-202.560564571109,92.6104102417814,4.978063951848));
#21164=CARTESIAN_POINT('Ctrl Pts',(-201.670020777333,95.7564540970319,5.13697227065231));
#21165=CARTESIAN_POINT('Ctrl Pts',(-203.832364716408,98.2089892908554,5.29588058945662));
#21166=CARTESIAN_POINT('Ctrl Pts',(-207.065183633062,97.7195589690321,5.45478890826092));
#21167=CARTESIAN_POINT('Ctrl Pts',(-208.404665277056,94.7368673803487,5.61369722706523));
#21168=CARTESIAN_POINT('Ctrl Pts',(-206.622787848284,91.9954128363827,5.77260554586954));
#21169=CARTESIAN_POINT('Ctrl Pts',(-203.35315665777,92.0085302223715,5.93151386467384));
#21170=CARTESIAN_POINT('Ctrl Pts',(-201.593333036985,94.7641936654509,6.09042218347815));
#21171=CARTESIAN_POINT('Ctrl Pts',(-202.95670361228,97.7360417204863,6.24933050228246));
#21172=CARTESIAN_POINT('Ctrl Pts',(-206.193345478335,98.1995173063525,6.40823882108676));
#21173=CARTESIAN_POINT('Ctrl Pts',(-208.335941547629,95.7297111860981,6.56714713989107));
#21174=CARTESIAN_POINT('Ctrl Pts',(-207.420183691185,92.59091400626,6.72605545869537));
#21175=CARTESIAN_POINT('Ctrl Pts',(-204.285628476556,91.6607399396267,6.88496377749968));
#21176=CARTESIAN_POINT('Ctrl Pts',(-201.806001090237,93.7919621741243,7.04387209630399));
#21177=CARTESIAN_POINT('Ctrl Pts',(-202.254596205724,97.0306999853957,7.2027804151083));
#21178=CARTESIAN_POINT('Ctrl Pts',(-205.220146834992,98.4077147467702,7.3616887339126));
#21179=CARTESIAN_POINT('Ctrl Pts',(-207.983869306475,96.6605747156291,7.52059705271691));
#21180=CARTESIAN_POINT('Ctrl Pts',(-208.012013747872,93.3910383450994,7.67950537152122));
#21181=CARTESIAN_POINT('Ctrl Pts',(-205.278777649875,91.5965800367509,7.83841369032552));
#21182=CARTESIAN_POINT('Ctrl Pts',(-202.289961318312,92.9223391113879,7.99732200912983));
#21183=CARTESIAN_POINT('Ctrl Pts',(-201.785678160579,96.1528744671184,8.15623032793414));
#21184=CARTESIAN_POINT('Ctrl Pts',(-204.228249339416,98.3264673968342,8.31513864673844));
#21185=CARTESIAN_POINT('Ctrl Pts',(-207.378352898179,97.4503921963708,8.47404696554275));
#21186=CARTESIAN_POINT('Ctrl Pts',(-208.34800910225,94.3278248178017,8.63295528434706));
#21187=CARTESIAN_POINT('Ctrl Pts',(-206.248247981384,91.8215001335089,8.79186360315136));
#21188=CARTESIAN_POINT('Ctrl Pts',(-203.004107062594,92.2291886013793,8.95077192195567));
#21189=CARTESIAN_POINT('Ctrl Pts',(-201.589778481136,95.1771259907191,9.10968024075998));
#21190=CARTESIAN_POINT('Ctrl Pts',(-203.301902872831,97.9626762514681,9.26858855956428));
#21191=CARTESIAN_POINT('Ctrl Pts',(-206.570823731434,98.0320780380912,9.42749687836859));
#21192=CARTESIAN_POINT('Ctrl Pts',(-208.399630949831,95.3217045683015,9.5864051971729));
#21193=CARTESIAN_POINT('Ctrl Pts',(-207.111694510394,92.3163959459186,9.7453135159772));
#21194=CARTESIAN_POINT('Ctrl Pts',(-203.887780145802,91.7713855262297,9.90422183478152));
#21195=CARTESIAN_POINT('Ctrl Pts',(-201.683536512486,94.1863327705371,10.0631301535858));
#21196=CARTESIAN_POINT('Ctrl Pts',(-202.519789537097,97.3472410366256,10.2220384723901));
#21197=CARTESIAN_POINT('Ctrl Pts',(-205.629871793297,98.3562249549636,10.3809467911944));
#21198=CARTESIAN_POINT('Ctrl Pts',(-208.16249462935,96.2882593464234,10.5398551099987));
#21199=CARTESIAN_POINT('Ctrl Pts',(-207.795777735762,93.0392319676905,10.698763428803));
#21200=CARTESIAN_POINT('Ctrl Pts',(-204.865923061858,91.5878148058802,10.8576717476073));
#21201=CARTESIAN_POINT('Ctrl Pts',(-202.058988626292,93.2646508927504,11.0165800664117));
#21202=CARTESIAN_POINT('Ctrl Pts',(-201.948340547065,96.5324356455089,11.175488385216));
#21203=CARTESIAN_POINT('Ctrl Pts',(-204.635419746522,98.3953005261812,11.3343967040203));
#21204=CARTESIAN_POINT('Ctrl Pts',(-207.65674204753,97.1453918330226,11.4933050228246));
#21205=CARTESIAN_POINT('Ctrl Pts',(-208.242392933218,93.9286118859498,11.6522133416289));
#21206=CARTESIAN_POINT('Ctrl Pts',(-205.855454217288,91.6940685871547,11.8111216604332));
#21207=CARTESIAN_POINT('Ctrl Pts',(-202.684244636183,92.4903662579446,11.9700299792375));
#21208=CARTESIAN_POINT('Ctrl Pts',(-201.636093689906,95.5874680937925,12.1289382980418));
#21209=CARTESIAN_POINT('Ctrl Pts',(-203.671934451039,98.145985747263,12.2878466168461));
#21210=CARTESIAN_POINT('Ctrl Pts',(-206.925330863944,97.8202988296705,12.4467549356504));
#21211=CARTESIAN_POINT('Ctrl Pts',(-208.413605459812,94.9089934669425,12.6056632544547));
#21212=CARTESIAN_POINT('Ctrl Pts',(-206.772324723283,92.0811218765405,12.764571573259));
#21213=CARTESIAN_POINT('Ctrl Pts',(-203.506196489364,91.9292451260705,12.9234798920633));
#21214=CARTESIAN_POINT('Ctrl Pts',(-201.609570618045,94.5926021227402,13.0823882108676));
#21215=CARTESIAN_POINT('Ctrl Pts',(-202.821252510011,97.6294569400588,13.241296529672));
#21216=CARTESIAN_POINT('Ctrl Pts',(-206.030385749313,98.2556550232583,13.4002048484762));
#21217=CARTESIAN_POINT('Ctrl Pts',(-208.29487285021,95.8971049696819,13.5591131672806));
#21218=CARTESIAN_POINT('Ctrl Pts',(-207.538657347822,92.7160991050779,13.7180214860849));
#21219=CARTESIAN_POINT('Ctrl Pts',(-204.455029163672,91.6289480575171,13.8769298048892));
#21220=CARTESIAN_POINT('Ctrl Pts',(-201.871024149848,93.6323397465202,14.0358381236935));
#21221=CARTESIAN_POINT('Ctrl Pts',(-202.155629226407,96.8895870838205,14.1947464424978));
#21222=CARTESIAN_POINT('Ctrl Pts',(-205.047921631297,98.4144820733316,14.3536547613021));
#21223=CARTESIAN_POINT('Ctrl Pts',(-207.896280032535,96.8090181206517,14.5125630801064));
#21224=CARTESIAN_POINT('Ctrl Pts',(-208.089361245615,93.5450664505984,14.6714713989107));
#21225=CARTESIAN_POINT('Ctrl Pts',(-205.450150650489,91.6149818522251,14.830379717715));
#21226=CARTESIAN_POINT('Ctrl Pts',(-202.398246861444,92.7882435307288,14.9892880365193));
#21227=CARTESIAN_POINT('Ctrl Pts',(-201.731601495486,95.9892199101742,15.1481963553236));
#21228=CARTESIAN_POINT('Ctrl Pts',(-204.06138688326,98.2832882782678,15.3071046741279));
#21229=CARTESIAN_POINT('Ctrl Pts',(-207.251683247105,97.5672793094413,15.4660129929322));
#21230=CARTESIAN_POINT('Ctrl Pts',(-208.377659589143,94.4976077296224,15.6249213117366));
#21231=CARTESIAN_POINT('Ctrl Pts',(-206.407039480148,91.8885436856663,15.7838296305408));
#21232=CARTESIAN_POINT('Ctrl Pts',(-203.146452807187,92.1319868369347,15.9427379493452));
#21233=CARTESIAN_POINT('Ctrl Pts',(-201.585195046037,95.0048775319451,16.1016462681495));
#21234=CARTESIAN_POINT('Ctrl Pts',(-203.154555992253,97.8731205591728,16.2605545869538));
#21235=CARTESIAN_POINT('Ctrl Pts',(-206.415874445363,98.1076826331683,16.4194629057581));
#21236=CARTESIAN_POINT('Ctrl Pts',(-208.378979897898,95.4924036763794,16.5783712245624));
#21237=CARTESIAN_POINT('Ctrl Pts',(-207.24459570974,92.4272494613622,16.7372795433667));
#21238=CARTESIAN_POINT('Ctrl Pts',(-204.051739039702,91.7175333660049,16.896187862171));
#21239=CARTESIAN_POINT('Ctrl Pts',(-201.729695205268,94.0237806550419,17.0550961809753));
#21240=CARTESIAN_POINT('Ctrl Pts',(-202.180151203454,96.1462649533788,17.1610350601782));
#21241=CARTESIAN_POINT('Ctrl Pts',(-202.804802895981,96.8768634390787,17.2140044997796));
#21242=CARTESIAN_POINT('Ctrl Pts',(-204.301933573839,92.3888678140614,-0.214004499779623));
#21243=CARTESIAN_POINT('Ctrl Pts',(-203.43290490324,92.6211960514381,-0.161035060178187));
#21244=CARTESIAN_POINT('Ctrl Pts',(-201.960390383187,94.0193135754141,-0.0550961809753161));
#21245=CARTESIAN_POINT('Ctrl Pts',(-202.528670089889,97.0288354900421,0.103812137828991));
#21246=CARTESIAN_POINT('Ctrl Pts',(-205.367278697187,98.1739996853001,0.262720456633297));
#21247=CARTESIAN_POINT('Ctrl Pts',(-207.866954658562,96.4114223759756,0.421628775437604));
#21248=CARTESIAN_POINT('Ctrl Pts',(-207.73931073102,93.3538399688327,0.58053709424191));
#21249=CARTESIAN_POINT('Ctrl Pts',(-205.099778896544,91.8059366529208,0.739445413046218));
#21250=CARTESIAN_POINT('Ctrl Pts',(-202.369021659162,93.1860740882583,0.898353731850525));
#21251=CARTESIAN_POINT('Ctrl Pts',(-202.050194660526,96.2293150144601,1.05726205065483));
#21252=CARTESIAN_POINT('Ctrl Pts',(-204.435774899398,98.1454773300738,1.21617036945914));
#21253=CARTESIAN_POINT('Ctrl Pts',(-207.338602024967,97.1779284398204,1.37507868826344));
#21254=CARTESIAN_POINT('Ctrl Pts',(-208.09743867911,94.2136659155149,1.53398700706775));
#21255=CARTESIAN_POINT('Ctrl Pts',(-206.016571531969,91.9703120675979,1.69289532587206));
#21256=CARTESIAN_POINT('Ctrl Pts',(-203.003726177937,92.504539169652,1.85180364467636));
#21257=CARTESIAN_POINT('Ctrl Pts',(-201.821040798587,95.3265783615671,2.01071196348067));
#21258=CARTESIAN_POINT('Ctrl Pts',(-203.55279043592,97.8492134400937,2.16962028228498));
#21259=CARTESIAN_POINT('Ctrl Pts',(-206.611325262991,97.7597218308491,2.32852860108929));
#21260=CARTESIAN_POINT('Ctrl Pts',(-208.1926152742,95.1401479230941,2.48743691989359));
#21261=CARTESIAN_POINT('Ctrl Pts',(-206.84695120019,92.3920880475125,2.6463452386979));
#21262=CARTESIAN_POINT('Ctrl Pts',(-203.808022949968,92.0349326623793,2.80525355750221));
#21263=CARTESIAN_POINT('Ctrl Pts',(-201.86188591684,94.3961178915378,2.96416187630651));
#21264=CARTESIAN_POINT('Ctrl Pts',(-202.792736810723,97.3109354790277,3.12307019511082));
#21265=CARTESIAN_POINT('Ctrl Pts',(-205.747181921757,98.1071132526631,3.28197851391513));
#21266=CARTESIAN_POINT('Ctrl Pts',(-208.016619000273,96.0547243216571,3.44088683271943));
#21267=CARTESIAN_POINT('Ctrl Pts',(-207.520453494377,93.0353759220375,3.59979515152374));
#21268=CARTESIAN_POINT('Ctrl Pts',(-204.71356439595,91.8171729183909,3.75870347032804));
#21269=CARTESIAN_POINT('Ctrl Pts',(-202.16927625763,93.5169502096079,3.91761178913235));
#21270=CARTESIAN_POINT('Ctrl Pts',(-202.220164008024,96.5763709727973,4.07652010793666));
#21271=CARTESIAN_POINT('Ctrl Pts',(-204.81957432615,98.1905924469556,4.23542842674096));
#21272=CARTESIAN_POINT('Ctrl Pts',(-207.58439688551,96.8797144263097,4.39433674554527));
#21273=CARTESIAN_POINT('Ctrl Pts',(-207.97987326549,93.8455352288158,4.55324506434958));
#21274=CARTESIAN_POINT('Ctrl Pts',(-205.643435141103,91.8697564303231,4.71215338315388));
#21275=CARTESIAN_POINT('Ctrl Pts',(-202.717102870891,92.7637499504281,4.87106170195819));
#21276=CARTESIAN_POINT('Ctrl Pts',(-201.883705173178,95.7079125218746,5.0299700207625));
#21277=CARTESIAN_POINT('Ctrl Pts',(-203.907291742512,98.0030688054592,5.18887833956681));
#21278=CARTESIAN_POINT('Ctrl Pts',(-206.932661029337,97.5450451728775,5.34778665837111));
#21279=CARTESIAN_POINT('Ctrl Pts',(-208.186188285418,94.7537525712456,5.50669497717542));
#21280=CARTESIAN_POINT('Ctrl Pts',(-206.518653732796,92.1882168600391,5.66560329597973));
#21281=CARTESIAN_POINT('Ctrl Pts',(-203.458834411625,92.20049250483,5.82451161478403));
#21282=CARTESIAN_POINT('Ctrl Pts',(-201.811938476587,94.7793253316762,5.98341993358834));
#21283=CARTESIAN_POINT('Ctrl Pts',(-203.08782171391,97.5604702280067,6.14232825239264));
#21284=CARTESIAN_POINT('Ctrl Pts',(-206.116768631898,97.9942046371468,6.30123657119695));
#21285=CARTESIAN_POINT('Ctrl Pts',(-208.121874550055,95.6828857005571,6.46014489000126));
#21286=CARTESIAN_POINT('Ctrl Pts',(-207.264880773267,92.7455047861689,6.61905320880557));
#21287=CARTESIAN_POINT('Ctrl Pts',(-204.331469617653,91.8750198857941,6.77796152760987));
#21288=CARTESIAN_POINT('Ctrl Pts',(-202.010959644548,93.8694818268668,6.93686984641418));
#21289=CARTESIAN_POINT('Ctrl Pts',(-202.430768461436,96.9003901935,7.09577816521848));
#21290=CARTESIAN_POINT('Ctrl Pts',(-205.206020037109,98.1890420710008,7.25468648402279));
#21291=CARTESIAN_POINT('Ctrl Pts',(-207.792394745404,96.5540158210718,7.4135948028271));
#21292=CARTESIAN_POINT('Ctrl Pts',(-207.818733161131,93.494285235298,7.5725031216314));
#21293=CARTESIAN_POINT('Ctrl Pts',(-205.260888519131,91.8149771167401,7.73141144043572));
#21294=CARTESIAN_POINT('Ctrl Pts',(-202.463864198688,93.0556623792128,7.89031975924001));
#21295=CARTESIAN_POINT('Ctrl Pts',(-201.991940835023,96.0788946409636,8.04922807804433));
#21296=CARTESIAN_POINT('Ctrl Pts',(-204.277772493353,98.1130083544613,8.20813639684863));
#21297=CARTESIAN_POINT('Ctrl Pts',(-207.22573425759,97.2931508020396,8.36704471565294));
#21298=CARTESIAN_POINT('Ctrl Pts',(-208.13316773104,94.3709582243806,8.52595303445724));
#21299=CARTESIAN_POINT('Ctrl Pts',(-206.168148047441,92.0254641159393,8.68486135326156));
#21300=CARTESIAN_POINT('Ctrl Pts',(-203.132183290097,92.4069912602325,8.84376967206585));
#21301=CARTESIAN_POINT('Ctrl Pts',(-201.808612016192,95.1657598356219,9.00267799087017));
#21302=CARTESIAN_POINT('Ctrl Pts',(-203.410869576358,97.7725616463765,9.16158630967448));
#21303=CARTESIAN_POINT('Ctrl Pts',(-206.470024147537,97.8375099280815,9.32049462847878));
#21304=CARTESIAN_POINT('Ctrl Pts',(-208.18147701041,95.3010608219831,9.47940294728308));
#21305=CARTESIAN_POINT('Ctrl Pts',(-206.97618730885,92.4886025191853,9.63831126608739));
#21306=CARTESIAN_POINT('Ctrl Pts',(-203.959151169973,91.9785653574278,9.7972195848917));
#21307=CARTESIAN_POINT('Ctrl Pts',(-201.896353605112,94.2385457060304,9.95612790369601));
#21308=CARTESIAN_POINT('Ctrl Pts',(-202.678944366271,97.1966188407269,10.1150362225003));
#21309=CARTESIAN_POINT('Ctrl Pts',(-205.589452990473,98.1408563733998,10.2739445413046));
#21310=CARTESIAN_POINT('Ctrl Pts',(-207.959557701204,96.2055918876419,10.4328528601089));
#21311=CARTESIAN_POINT('Ctrl Pts',(-207.616372989835,93.1650542339453,10.5917611789132));
#21312=CARTESIAN_POINT('Ctrl Pts',(-204.874526764046,91.8067743497581,10.7506694977175));
#21313=CARTESIAN_POINT('Ctrl Pts',(-202.247712998591,93.3760080516899,10.9095778165218));
#21314=CARTESIAN_POINT('Ctrl Pts',(-202.144165194284,96.43409942081,11.0684861353261));
#21315=CARTESIAN_POINT('Ctrl Pts',(-204.658814820783,98.1774244695644,11.2273944541305));
#21316=CARTESIAN_POINT('Ctrl Pts',(-207.486259206231,97.0077222780384,11.3863027729348));
#21317=CARTESIAN_POINT('Ctrl Pts',(-208.034328939812,93.9973627419037,11.5452110917391));
#21318=CARTESIAN_POINT('Ctrl Pts',(-205.80055981544,91.9062098377222,11.7041194105434));
#21319=CARTESIAN_POINT('Ctrl Pts',(-202.832846399964,92.6514091756644,11.8630277293477));
#21320=CARTESIAN_POINT('Ctrl Pts',(-201.851955183173,95.5497703316425,12.021936048152));
#21321=CARTESIAN_POINT('Ctrl Pts',(-203.757156269404,97.9441081922421,12.1808443669563));
#21322=CARTESIAN_POINT('Ctrl Pts',(-206.801782596837,97.6393205678785,12.3397526857606));
#21323=CARTESIAN_POINT('Ctrl Pts',(-208.194554777643,94.914833346033,12.4986610045649));
#21324=CARTESIAN_POINT('Ctrl Pts',(-206.658594843181,92.2684259606358,12.6575693233692));
#21325=CARTESIAN_POINT('Ctrl Pts',(-203.60205369427,92.1262951243283,12.8164776421735));
#21326=CARTESIAN_POINT('Ctrl Pts',(-201.827134093879,94.6187447991505,12.9753859609778));
#21327=CARTESIAN_POINT('Ctrl Pts',(-202.961062493788,97.4607249810683,13.1342942797821));
#21328=CARTESIAN_POINT('Ctrl Pts',(-205.964266010537,98.046740003011,13.2932025985864));
#21329=CARTESIAN_POINT('Ctrl Pts',(-208.083441226376,95.8395378436917,13.4521109173908));
#21330=CARTESIAN_POINT('Ctrl Pts',(-207.375751988553,92.8626567711379,13.6110192361951));
#21331=CARTESIAN_POINT('Ctrl Pts',(-204.489999881544,91.8452680852187,13.7699275549994));
#21332=CARTESIAN_POINT('Ctrl Pts',(-202.071810181666,93.7201023526643,13.9288358738037));
#21333=CARTESIAN_POINT('Ctrl Pts',(-202.33815218216,96.7683324911026,14.087744192608));
#21334=CARTESIAN_POINT('Ctrl Pts',(-205.044846505554,98.1953751389704,14.2466525114123));
#21335=CARTESIAN_POINT('Ctrl Pts',(-207.710426065418,96.6929336293271,14.4055608302166));
#21336=CARTESIAN_POINT('Ctrl Pts',(-207.891117278559,93.6384293744216,14.5644691490209));
#21337=CARTESIAN_POINT('Ctrl Pts',(-205.421264533382,91.8321980897649,14.7233774678252));
#21338=CARTESIAN_POINT('Ctrl Pts',(-202.565201070578,92.9301716970297,14.8822857866295));
#21339=CARTESIAN_POINT('Ctrl Pts',(-201.941334263506,95.9257417787117,15.0411941054338));
#21340=CARTESIAN_POINT('Ctrl Pts',(-204.121617582424,98.0726000351243,15.2001024242381));
#21341=CARTESIAN_POINT('Ctrl Pts',(-207.107192983917,97.4025372820827,15.3590107430424));
#21342=CARTESIAN_POINT('Ctrl Pts',(-208.160915549491,94.5298461856591,15.5179190618468));
#21343=CARTESIAN_POINT('Ctrl Pts',(-206.316749913415,92.0882054908218,15.676827380651));
#21344=CARTESIAN_POINT('Ctrl Pts',(-203.265394724113,92.3160269221865,15.8357356994554));
#21345=CARTESIAN_POINT('Ctrl Pts',(-201.804322699612,95.0045645412634,15.9946440182597));
#21346=CARTESIAN_POINT('Ctrl Pts',(-203.272977928696,97.6887527328817,16.153552337064));
#21347=CARTESIAN_POINT('Ctrl Pts',(-206.325017939896,97.9082629847128,16.3124606558683));
#21348=CARTESIAN_POINT('Ctrl Pts',(-208.16215113418,95.4608061873071,16.4713689746726));
#21349=CARTESIAN_POINT('Ctrl Pts',(-207.100560253035,92.5923425768892,16.6302772934769));
#21350=CARTESIAN_POINT('Ctrl Pts',(-204.112588839912,91.9281688843269,16.7891856122812));
#21351=CARTESIAN_POINT('Ctrl Pts',(-201.939550299719,94.0864245416824,16.9480939310855));
#21352=CARTESIAN_POINT('Ctrl Pts',(-202.36110058667,96.0727092589846,17.0540328102884));
#21353=CARTESIAN_POINT('Ctrl Pts',(-202.945668449658,96.7564253212268,17.1070022498898));
#21354=CARTESIAN_POINT('Ctrl Pts',(-204.349800002025,92.5679131979649,-0.321006749669433));
#21355=CARTESIAN_POINT('Ctrl Pts',(-203.540360643981,92.7843106836636,-0.268037310067998));
#21356=CARTESIAN_POINT('Ctrl Pts',(-202.168816472716,94.0865592622945,-0.162098430865127));
#21357=CARTESIAN_POINT('Ctrl Pts',(-202.698129229066,96.8897182017072,-0.00319011206082008));
#21358=CARTESIAN_POINT('Ctrl Pts',(-205.3420943899,97.9563584662055,0.155718206743487));
#21359=CARTESIAN_POINT('Ctrl Pts',(-207.670367522821,96.3146411166748,0.314626525547793));
#21360=CARTESIAN_POINT('Ctrl Pts',(-207.55147614183,93.4667171936373,0.4735348443521));
#21361=CARTESIAN_POINT('Ctrl Pts',(-205.092937055701,92.0249536376869,0.632443163156407));
#21362=CARTESIAN_POINT('Ctrl Pts',(-202.549427894286,93.3104550227009,0.791351481960713));
#21363=CARTESIAN_POINT('Ctrl Pts',(-202.252462869042,96.1450208604193,0.950259800765021));
#21364=CARTESIAN_POINT('Ctrl Pts',(-204.474463825331,97.9297918894226,1.10916811956933));
#21365=CARTESIAN_POINT('Ctrl Pts',(-207.178244039411,97.0285878450691,1.26807643837364));
#21366=CARTESIAN_POINT('Ctrl Pts',(-207.885047249673,94.2675848587194,1.42698475717794));
#21367=CARTESIAN_POINT('Ctrl Pts',(-205.946865202589,92.1780578270374,1.58589307598225));
#21368=CARTESIAN_POINT('Ctrl Pts',(-203.140610712076,92.6756529664916,1.74480139478655));
#21369=CARTESIAN_POINT('Ctrl Pts',(-202.039022091796,95.3041848770717,1.90370971359086));
#21370=CARTESIAN_POINT('Ctrl Pts',(-203.652025623394,97.6538428200417,2.06261803239516));
#21371=CARTESIAN_POINT('Ctrl Pts',(-206.500836658906,97.5704876521536,2.22152635119947));
#21372=CARTESIAN_POINT('Ctrl Pts',(-207.973697583819,95.1305379773285,2.38043467000378));
#21373=CARTESIAN_POINT('Ctrl Pts',(-206.720305721087,92.5709126199468,2.53934298880809));
#21374=CARTESIAN_POINT('Ctrl Pts',(-203.889756839074,92.2382473863993,2.6982513076124));
#21375=CARTESIAN_POINT('Ctrl Pts',(-202.077066459509,94.4375260992589,2.8571596264167));
#21376=CARTESIAN_POINT('Ctrl Pts',(-202.944088889806,97.1524745890555,3.01606794522101));
#21377=CARTESIAN_POINT('Ctrl Pts',(-205.695947643099,97.8940584375333,3.17497626402531));
#21378=CARTESIAN_POINT('Ctrl Pts',(-207.80976937776,95.9824018547592,3.33388458282962));
#21379=CARTESIAN_POINT('Ctrl Pts',(-207.347625950087,93.1700902326187,3.49279290163393));
#21380=CARTESIAN_POINT('Ctrl Pts',(-204.733205290795,92.0354194322189,3.65170122043824));
#21381=CARTESIAN_POINT('Ctrl Pts',(-202.363379038756,93.6186429620847,3.81060953924254));
#21382=CARTESIAN_POINT('Ctrl Pts',(-202.410777415132,96.4682791850591,3.96951785804685));
#21383=CARTESIAN_POINT('Ctrl Pts',(-204.831946118055,97.9718134618773,4.12842617685115));
#21384=CARTESIAN_POINT('Ctrl Pts',(-207.407184741668,96.7508223721654,4.28733449565546));
#21385=CARTESIAN_POINT('Ctrl Pts',(-207.775543298713,93.9246969002444,4.44624281445977));
#21386=CARTESIAN_POINT('Ctrl Pts',(-205.599314781178,92.0843972917328,4.60515113326408));
#21387=CARTESIAN_POINT('Ctrl Pts',(-202.873641170674,92.9170896590748,4.76405945206838));
#21388=CARTESIAN_POINT('Ctrl Pts',(-202.097389569024,95.6593709467175,4.92296777087269));
#21389=CARTESIAN_POINT('Ctrl Pts',(-203.982218768616,97.7971483200629,5.08187608967699));
#21390=CARTESIAN_POINT('Ctrl Pts',(-206.800138425611,97.3705313767228,5.24078440848131));
#21391=CARTESIAN_POINT('Ctrl Pts',(-207.96771129378,94.7706377621425,5.3996927272856));
#21392=CARTESIAN_POINT('Ctrl Pts',(-206.414519617308,92.3810208836956,5.55860104608992));
#21393=CARTESIAN_POINT('Ctrl Pts',(-203.564512165481,92.3924547872884,5.71750936489422));
#21394=CARTESIAN_POINT('Ctrl Pts',(-202.03054391619,94.7944569979015,5.87641768369853));
#21395=CARTESIAN_POINT('Ctrl Pts',(-203.21893981554,97.3848987355268,6.03532600250283));
#21396=CARTESIAN_POINT('Ctrl Pts',(-206.040191785461,97.7888919679414,6.19423432130714));
#21397=CARTESIAN_POINT('Ctrl Pts',(-207.90780755248,95.6360602150159,6.35314264011145));
#21398=CARTESIAN_POINT('Ctrl Pts',(-207.10957785535,92.9000955660777,6.51205095891575));
#21399=CARTESIAN_POINT('Ctrl Pts',(-204.37731075875,92.0892998319615,6.67095927772006));
#21400=CARTESIAN_POINT('Ctrl Pts',(-202.215918198859,93.9470014796092,6.82986759652437));
#21401=CARTESIAN_POINT('Ctrl Pts',(-202.606940717148,96.7700804016044,6.98877591532868));
#21402=CARTESIAN_POINT('Ctrl Pts',(-205.191893239227,97.9703693952313,7.14768423413298));
#21403=CARTESIAN_POINT('Ctrl Pts',(-207.600920184333,96.4474569265149,7.30659255293729));
#21404=CARTESIAN_POINT('Ctrl Pts',(-207.62545257439,93.5975321254964,7.46550087174159));
#21405=CARTESIAN_POINT('Ctrl Pts',(-205.242999388387,92.0333741967293,7.6244091905459));
#21406=CARTESIAN_POINT('Ctrl Pts',(-202.637767079064,93.1889856470376,7.7833175093502));
#21407=CARTESIAN_POINT('Ctrl Pts',(-202.198203509467,96.0049148148089,7.94222582815452));
#21408=CARTESIAN_POINT('Ctrl Pts',(-204.32729564729,97.8995493120883,8.10113414695882));
#21409=CARTESIAN_POINT('Ctrl Pts',(-207.073115617,97.1359094077086,8.26004246576313));
#21410=CARTESIAN_POINT('Ctrl Pts',(-207.91832635983,94.4140916309592,8.41895078456744));
#21411=CARTESIAN_POINT('Ctrl Pts',(-206.088048113498,92.22942809837,8.57785910337174));
#21412=CARTESIAN_POINT('Ctrl Pts',(-203.2602595176,92.5847939190855,8.73676742217605));
#21413=CARTESIAN_POINT('Ctrl Pts',(-202.027445551247,95.1543936805248,8.89567574098035));
#21414=CARTESIAN_POINT('Ctrl Pts',(-203.519836279884,97.5824470412848,9.05458405978466));
#21415=CARTESIAN_POINT('Ctrl Pts',(-206.36922456364,97.6429418180719,9.21349237858896));
#21416=CARTESIAN_POINT('Ctrl Pts',(-207.96332307099,95.2804170756647,9.37240069739328));
#21417=CARTESIAN_POINT('Ctrl Pts',(-206.840680107306,92.6608090924519,9.53130901619758));
#21418=CARTESIAN_POINT('Ctrl Pts',(-204.030522194145,92.185745188626,9.69021733500189));
#21419=CARTESIAN_POINT('Ctrl Pts',(-202.109170697738,94.2907586415236,9.8491256538062));
#21420=CARTESIAN_POINT('Ctrl Pts',(-202.838099195444,97.0459966448283,10.0080339726105));
#21421=CARTESIAN_POINT('Ctrl Pts',(-205.549034187648,97.9254877918359,10.1669422914148));
#21422=CARTESIAN_POINT('Ctrl Pts',(-207.756620773058,96.1229244288606,10.3258506102191));
#21423=CARTESIAN_POINT('Ctrl Pts',(-207.436968243909,93.2908765001999,10.4847589290234));
#21424=CARTESIAN_POINT('Ctrl Pts',(-204.883130466234,92.0257338936362,10.6436672478277));
#21425=CARTESIAN_POINT('Ctrl Pts',(-202.436437370889,93.4873652106293,10.802575566632));
#21426=CARTESIAN_POINT('Ctrl Pts',(-202.339989841504,96.3357631961111,10.9614838854363));
#21427=CARTESIAN_POINT('Ctrl Pts',(-204.682209895044,97.9595484129476,11.1203922042407));
#21428=CARTESIAN_POINT('Ctrl Pts',(-207.315776364933,96.8700527230541,11.279300523045));
#21429=CARTESIAN_POINT('Ctrl Pts',(-207.826264946406,94.0661135978575,11.4382088418493));
#21430=CARTESIAN_POINT('Ctrl Pts',(-205.745665413592,92.1183510882897,11.5971171606536));
#21431=CARTESIAN_POINT('Ctrl Pts',(-202.981448163745,92.8124520933842,11.7560254794579));
#21432=CARTESIAN_POINT('Ctrl Pts',(-202.06781667644,95.5120725694926,11.9149337982622));
#21433=CARTESIAN_POINT('Ctrl Pts',(-203.842378087768,97.7422306372212,12.0738421170665));
#21434=CARTESIAN_POINT('Ctrl Pts',(-206.678234329729,97.4583423060864,12.2327504358708));
#21435=CARTESIAN_POINT('Ctrl Pts',(-207.975504095473,94.9206732251237,12.3916587546751));
#21436=CARTESIAN_POINT('Ctrl Pts',(-206.544864963079,92.455730044731,12.5505670734794));
#21437=CARTESIAN_POINT('Ctrl Pts',(-203.697910899177,92.3233451225861,12.7094753922837));
#21438=CARTESIAN_POINT('Ctrl Pts',(-202.044697569714,94.6448874755608,12.868383711088));
#21439=CARTESIAN_POINT('Ctrl Pts',(-203.100872477565,97.2919930220778,13.0272920298923));
#21440=CARTESIAN_POINT('Ctrl Pts',(-205.898146271762,97.837824982764,13.1862003486966));
#21441=CARTESIAN_POINT('Ctrl Pts',(-207.872009602541,95.7819707177012,13.3451086675009));
#21442=CARTESIAN_POINT('Ctrl Pts',(-207.212846629283,93.009214437198,13.5040169863053));
#21443=CARTESIAN_POINT('Ctrl Pts',(-204.524970599415,92.0615881129203,13.6629253051095));
#21444=CARTESIAN_POINT('Ctrl Pts',(-202.272596213484,93.8078649588083,13.8218336239139));
#21445=CARTESIAN_POINT('Ctrl Pts',(-202.520675137913,96.6470778983847,13.9807419427182));
#21446=CARTESIAN_POINT('Ctrl Pts',(-205.041771379811,97.9762682046092,14.1396502615225));
#21447=CARTESIAN_POINT('Ctrl Pts',(-207.5245720983,96.5768491380024,14.2985585803268));
#21448=CARTESIAN_POINT('Ctrl Pts',(-207.692873311502,93.731792298245,14.4574668991311));
#21449=CARTESIAN_POINT('Ctrl Pts',(-205.392378416275,92.0494143273046,14.6163752179354));
#21450=CARTESIAN_POINT('Ctrl Pts',(-202.732155279711,93.0720998633307,14.7752835367397));
#21451=CARTESIAN_POINT('Ctrl Pts',(-202.151067031526,95.8622636472492,14.934191855544));
#21452=CARTESIAN_POINT('Ctrl Pts',(-204.181848281588,97.8619117919808,15.0931001743483));
#21453=CARTESIAN_POINT('Ctrl Pts',(-206.96270272073,97.237795254724,15.2520084931526));
#21454=CARTESIAN_POINT('Ctrl Pts',(-207.94417150984,94.5620846416957,15.4109168119569));
#21455=CARTESIAN_POINT('Ctrl Pts',(-206.226460346682,92.2878672959773,15.5698251307612));
#21456=CARTESIAN_POINT('Ctrl Pts',(-203.384336641039,92.5000670074382,15.7287334495655));
#21457=CARTESIAN_POINT('Ctrl Pts',(-202.023450353188,95.0042515505818,15.8876417683699));
#21458=CARTESIAN_POINT('Ctrl Pts',(-203.391399865139,97.5043849065904,16.0465500871742));
#21459=CARTESIAN_POINT('Ctrl Pts',(-206.234161434428,97.7088433362576,16.2054584059785));
#21460=CARTESIAN_POINT('Ctrl Pts',(-207.945322370463,95.4292086982347,16.3643667247828));
#21461=CARTESIAN_POINT('Ctrl Pts',(-206.956524796331,92.7574356924161,16.5232750435871));
#21462=CARTESIAN_POINT('Ctrl Pts',(-204.173438640123,92.1388044026488,16.6821833623914));
#21463=CARTESIAN_POINT('Ctrl Pts',(-202.14940539417,94.149068428323,16.8410916811957));
#21464=CARTESIAN_POINT('Ctrl Pts',(-202.542049969887,95.9991535645904,16.9470305603986));
#21465=CARTESIAN_POINT('Ctrl Pts',(-203.086534003335,96.6359872033749,17.));
#21466=CARTESIAN_POINT('Ctrl Pts',(-202.485814060779,95.0013541851486,0.887416697508031));
#21467=CARTESIAN_POINT('Ctrl Pts',(-202.484186185477,95.3337585357717,0.908364398593701));
#21468=CARTESIAN_POINT('Ctrl Pts',(-202.545408952213,95.6655886577545,0.929312099679371));
#21469=CARTESIAN_POINT('Ctrl Pts',(-202.672290532631,95.9700550589668,0.950259800765041));
#21470=CARTESIAN_POINT('Ctrl Pts',(-202.993129854472,96.7399445367538,1.00322924036648));
#21471=CARTESIAN_POINT('Ctrl Pts',(-203.733796839902,97.3348682130882,1.05619867996791));
#21472=CARTESIAN_POINT('Ctrl Pts',(-204.554760368296,97.4821293771965,1.10916811956935));
#21473=CARTESIAN_POINT('Ctrl Pts',(-205.375723896691,97.6293905413048,1.16213755917078));
#21474=CARTESIAN_POINT('Ctrl Pts',(-206.276983968051,97.3289891931869,1.21510699877222));
#21475=CARTESIAN_POINT('Ctrl Pts',(-206.845414538775,96.7186213547364,1.26807643837365));
#21476=CARTESIAN_POINT('Ctrl Pts',(-207.413845109498,96.1082535162859,1.32104587797509));
#21477=CARTESIAN_POINT('Ctrl Pts',(-207.649446179586,95.1879191875027,1.37401531757652));
#21478=CARTESIAN_POINT('Ctrl Pts',(-207.444216373449,94.3794975178307,1.42698475717796));
#21479=CARTESIAN_POINT('Ctrl Pts',(-207.238986567312,93.5710758481587,1.4799541967794));
#21480=CARTESIAN_POINT('Ctrl Pts',(-206.592925884951,92.8745668375981,1.53292363638083));
#21481=CARTESIAN_POINT('Ctrl Pts',(-205.802186462018,92.6092448555601,1.58589307598227));
#21482=CARTESIAN_POINT('Ctrl Pts',(-205.011447039085,92.3439228735221,1.6388625155837));
#21483=CARTESIAN_POINT('Ctrl Pts',(-204.07602887558,92.5097879200068,1.69183195518514));
#21484=CARTESIAN_POINT('Ctrl Pts',(-203.424721690448,93.0308090950125,1.74480139478657));
#21485=CARTESIAN_POINT('Ctrl Pts',(-202.840193630047,93.498409489736,1.79233982902706));
#21486=CARTESIAN_POINT('Ctrl Pts',(-202.484502970261,94.2520706545457,1.83987826326755));
#21487=CARTESIAN_POINT('Ctrl Pts',(-202.479323465531,95.0014637551426,1.88741669750803));
#21488=CARTESIAN_POINT('Ctrl Pts',(-204.206200717467,92.0307770462543,-1.66533453693773E-15));
#21489=CARTESIAN_POINT('Ctrl Pts',(-204.113164546597,92.0648100931486,-1.69173089419692E-15));
#21490=CARTESIAN_POINT('Ctrl Pts',(-204.022195753339,92.1036152875412,-1.82627024830213E-15));
#21491=CARTESIAN_POINT('Ctrl Pts',(-203.93350174438,92.146863146562,-1.76247905159244E-15));
#21492=CARTESIAN_POINT('Ctrl Pts',(-203.842828689001,92.1910760033496,-1.69726446968485E-15));
#21493=CARTESIAN_POINT('Ctrl Pts',(-203.754532399231,92.239932614376,-1.71252452587887E-15));
#21494=CARTESIAN_POINT('Ctrl Pts',(-203.668863408233,92.2931265192584,-1.74513181683267E-15));
#21495=CARTESIAN_POINT('Ctrl Pts',(-203.585834980389,92.3446808359581,-1.77673405788396E-15));
#21496=CARTESIAN_POINT('Ctrl Pts',(-203.505274053601,92.4003100531731,-2.01192529436932E-15));
#21497=CARTESIAN_POINT('Ctrl Pts',(-203.42744252456,92.4597659845155,-2.08166817117217E-15));
#21498=CARTESIAN_POINT('Ctrl Pts',(-203.359339936648,92.5117899244401,-2.14269318837466E-15));
#21499=CARTESIAN_POINT('Ctrl Pts',(-203.293327341741,92.5667444131619,-1.8186794360701E-15));
#21500=CARTESIAN_POINT('Ctrl Pts',(-203.229605551781,92.6244761991185,-1.81105130891979E-15));
#21501=CARTESIAN_POINT('Ctrl Pts',(-203.216356049157,92.6364802161122,-1.80946521269176E-15));
#21502=CARTESIAN_POINT('Ctrl Pts',(-203.20320393314,92.6486060983002,-8.45553191946793E-16));
#21503=CARTESIAN_POINT('Ctrl Pts',(-203.190167894587,92.6608364292545,-8.60422844084496E-16));
#21504=CARTESIAN_POINT('Ctrl Pts',(-203.117744720063,92.7287834048338,-9.43032864569248E-16));
#21505=CARTESIAN_POINT('Ctrl Pts',(-203.048787356972,92.800052338559,-1.63384023442941E-15));
#21506=CARTESIAN_POINT('Ctrl Pts',(-202.983534916614,92.8743511143521,-1.51267887105178E-15));
#21507=CARTESIAN_POINT('Ctrl Pts',(-202.918640599649,92.9482421179686,-1.39218247465811E-15));
#21508=CARTESIAN_POINT('Ctrl Pts',(-202.857410164585,93.0251305974732,-1.61166620503164E-15));
#21509=CARTESIAN_POINT('Ctrl Pts',(-202.800122429229,93.1047559605022,-1.70696790036118E-15));
#21510=CARTESIAN_POINT('Ctrl Pts',(-202.744171241289,93.1825236296888,-1.80004616629764E-15));
#21511=CARTESIAN_POINT('Ctrl Pts',(-202.691980644036,93.2629027086335,-1.49993186602241E-15));
#21512=CARTESIAN_POINT('Ctrl Pts',(-202.643857548798,93.3456645933452,-1.47104550762833E-15));
#21513=CARTESIAN_POINT('Ctrl Pts',(-202.623078179889,93.3814008593852,-1.45857248828985E-15));
#21514=CARTESIAN_POINT('Ctrl Pts',(-202.603057818574,93.4175815121137,-2.11179019747899E-15));
#21515=CARTESIAN_POINT('Ctrl Pts',(-202.58382418876,93.4541884794612,-2.15105711021124E-15));
#21516=CARTESIAN_POINT('Ctrl Pts',(-202.569909256858,93.480672479761,-2.17946549812013E-15));
#21517=CARTESIAN_POINT('Ctrl Pts',(-202.556406144173,93.5073796196226,-1.83372961098251E-15));
#21518=CARTESIAN_POINT('Ctrl Pts',(-202.543325986125,93.5343030584598,-1.87350135405495E-15));
#21519=CARTESIAN_POINT('Ctrl Pts',(-202.537164396374,93.5469857175079,-1.89223638490238E-15));
#21520=CARTESIAN_POINT('Ctrl Pts',(-202.53109884915,93.559711973925,-1.76798935478286E-15));
#21521=CARTESIAN_POINT('Ctrl Pts',(-202.525133507599,93.5724739887755,-1.76247905159244E-15));
#21522=CARTESIAN_POINT('Ctrl Pts',(-202.485117234082,93.6580832154258,-1.72551523355393E-15));
#21523=CARTESIAN_POINT('Ctrl Pts',(-202.449559207413,93.7453964352435,-1.29272896296815E-15));
#21524=CARTESIAN_POINT('Ctrl Pts',(-202.418711137482,93.8341759498457,-1.38777878078145E-15));
#21525=CARTESIAN_POINT('Ctrl Pts',(-202.388547297845,93.9209862769557,-1.48072033169087E-15));
#21526=CARTESIAN_POINT('Ctrl Pts',(-202.362886576913,94.0091992471836,-1.88906384068916E-15));
#21527=CARTESIAN_POINT('Ctrl Pts',(-202.342013489097,94.0986011792945,-1.97064586870965E-15));
#21528=CARTESIAN_POINT('Ctrl Pts',(-202.338634265004,94.1130748003348,-1.98385349554043E-15));
#21529=CARTESIAN_POINT('Ctrl Pts',(-202.335380633682,94.1275795899092,-2.29719255525669E-15));
#21530=CARTESIAN_POINT('Ctrl Pts',(-202.332253933038,94.1421146450262,-2.3037127760972E-15));
#21531=CARTESIAN_POINT('Ctrl Pts',(-202.312215536415,94.2352668948282,-2.34442810623525E-15));
#21532=CARTESIAN_POINT('Ctrl Pts',(-202.297386423123,94.3296632853158,-1.89809370242541E-15));
#21533=CARTESIAN_POINT('Ctrl Pts',(-202.287688012511,94.4248955183014,-1.88737914186277E-15));
#21534=CARTESIAN_POINT('Ctrl Pts',(-202.284332068712,94.4578487551403,-1.88367157940438E-15));
#21535=CARTESIAN_POINT('Ctrl Pts',(-202.281590899577,94.4909019448947,-1.99130593283213E-15));
#21536=CARTESIAN_POINT('Ctrl Pts',(-202.279462603563,94.5240376464396,-2.02615701994091E-15));
#21537=CARTESIAN_POINT('Ctrl Pts',(-202.278435428223,94.5400298652337,-2.04297713191284E-15));
#21538=CARTESIAN_POINT('Ctrl Pts',(-202.277551019282,94.5560412983696,-1.44883699021621E-15));
#21539=CARTESIAN_POINT('Ctrl Pts',(-202.276809217809,94.5720699538646,-1.4432899320127E-15));
#21540=CARTESIAN_POINT('Ctrl Pts',(-202.276232566489,94.5845300872998,-1.43897783700198E-15));
#21541=CARTESIAN_POINT('Ctrl Pts',(-202.275742191968,94.5969994802251,-1.93405229558996E-15));
#21542=CARTESIAN_POINT('Ctrl Pts',(-202.275338169858,94.6094673056919,-1.9151347174784E-15));
#21543=CARTESIAN_POINT('Ctrl Pts',(-202.272318849975,94.7026412989672,-1.77376072243412E-15));
#21544=CARTESIAN_POINT('Ctrl Pts',(-202.274110256434,94.7958785363416,-1.40451656878397E-15));
#21545=CARTESIAN_POINT('Ctrl Pts',(-202.280572703129,94.8888046622951,-1.47104550762833E-15));
#21546=CARTESIAN_POINT('Ctrl Pts',(-202.287048646371,94.9819248605413,-1.5377133893541E-15));
#21547=CARTESIAN_POINT('Ctrl Pts',(-202.298215544432,95.0747336270844,-1.60767188909222E-15));
#21548=CARTESIAN_POINT('Ctrl Pts',(-202.313983907893,95.166842280173,-1.69309011255336E-15));
#21549=CARTESIAN_POINT('Ctrl Pts',(-202.329531048883,95.2576586936497,-1.77730995987682E-15));
#21550=CARTESIAN_POINT('Ctrl Pts',(-202.34955191658,95.3477953472331,-1.39699777228343E-15));
#21551=CARTESIAN_POINT('Ctrl Pts',(-202.374003812269,95.4368545695215,-1.36002320516582E-15));
#21552=CARTESIAN_POINT('Ctrl Pts',(-202.383516754342,95.4715028124848,-1.34563835256958E-15));
#21553=CARTESIAN_POINT('Ctrl Pts',(-202.39370079569,95.5059876390941,-2.03473279209489E-15));
#21554=CARTESIAN_POINT('Ctrl Pts',(-202.404554992678,95.5402841682775,-2.05391259555654E-15));
#21555=CARTESIAN_POINT('Ctrl Pts',(-202.410353828332,95.5586070286854,-2.06415937182937E-15));
#21556=CARTESIAN_POINT('Ctrl Pts',(-202.4163439549,95.5768761294375,-1.49239684807345E-15));
#21557=CARTESIAN_POINT('Ctrl Pts',(-202.422525324126,95.5950875623995,-1.49880108324396E-15));
#21558=CARTESIAN_POINT('Ctrl Pts',(-202.428042981199,95.6113435791845,-1.50451767647659E-15));
#21559=CARTESIAN_POINT('Ctrl Pts',(-202.433713558872,95.6275548911267,-1.38447419983314E-15));
#21560=CARTESIAN_POINT('Ctrl Pts',(-202.439530699397,95.6437017576532,-1.41553435639707E-15));
#21561=CARTESIAN_POINT('Ctrl Pts',(-202.470363847948,95.7292865449133,-1.58016548698939E-15));
#21562=CARTESIAN_POINT('Ctrl Pts',(-202.505347385225,95.8131730030787,-1.91068776190809E-15));
#21563=CARTESIAN_POINT('Ctrl Pts',(-202.54441704991,95.8949805098665,-1.77635683940025E-15));
#21564=CARTESIAN_POINT('Ctrl Pts',(-202.575879531626,95.9608594265972,-1.66818124518231E-15));
#21565=CARTESIAN_POINT('Ctrl Pts',(-202.609992760709,96.025389849449,-1.40994256838161E-15));
#21566=CARTESIAN_POINT('Ctrl Pts',(-202.646741380164,96.0883553006046,-1.4432899320127E-15));
#21567=CARTESIAN_POINT('Ctrl Pts',(-202.66198370497,96.1144716519744,-1.4571215086927E-15));
#21568=CARTESIAN_POINT('Ctrl Pts',(-202.677679592969,96.1403185550972,-1.31270100888093E-15));
#21569=CARTESIAN_POINT('Ctrl Pts',(-202.693828681531,96.165879569832,-1.33226762955019E-15));
#21570=CARTESIAN_POINT('Ctrl Pts',(-202.702295555836,96.1792810629265,-1.3425262962934E-15));
#21571=CARTESIAN_POINT('Ctrl Pts',(-202.71088559022,96.1926016065556,-1.61636770759439E-15));
#21572=CARTESIAN_POINT('Ctrl Pts',(-202.719593926003,96.2058319566941,-1.60982338570648E-15));
#21573=CARTESIAN_POINT('Ctrl Pts',(-202.767002660722,96.2778588256104,-1.57419568048102E-15));
#21574=CARTESIAN_POINT('Ctrl Pts',(-202.817953855461,96.347277505506,-1.59581768743097E-15));
#21575=CARTESIAN_POINT('Ctrl Pts',(-202.872410801174,96.4137327204673,-1.22124532708767E-15));
#21576=CARTESIAN_POINT('Ctrl Pts',(-202.926867746887,96.4801879354285,-8.46672966744377E-16));
#21577=CARTESIAN_POINT('Ctrl Pts',(-202.984830774458,96.5436803772796,-3.7899909010744E-16));
#21578=CARTESIAN_POINT('Ctrl Pts',(-203.046292669322,96.6038107748045,-2.22044604925031E-16));
#21579=CARTESIAN_POINT('Ctrl Pts',(-203.058343445767,96.6156004858078,-1.91270685291611E-16));
#21580=CARTESIAN_POINT('Ctrl Pts',(-203.070528813095,96.6272607941278,-2.35826789791532E-16));
#21581=CARTESIAN_POINT('Ctrl Pts',(-203.082846187392,96.6387906377555,-2.22044604925031E-16));
#21582=CARTESIAN_POINT('Origin',(-205.,95.,9.));
#21583=CARTESIAN_POINT('Origin',(-205.,65.,18.));
#21584=CARTESIAN_POINT('Origin',(-205.,-95.,18.));
#21585=CARTESIAN_POINT('Origin',(-205.,-65.,18.));
#21586=CARTESIAN_POINT('Origin',(-205.,95.,18.));
#21587=CARTESIAN_POINT('Origin',(170.,-120.,0.));
#21588=CARTESIAN_POINT('',(170.,-120.,0.));
#21589=CARTESIAN_POINT('',(-170.,-120.,0.));
#21590=CARTESIAN_POINT('',(-170.,-120.,0.));
#21591=CARTESIAN_POINT('',(-170.,-120.,20.));
#21592=CARTESIAN_POINT('',(-170.,-120.,0.));
#21593=CARTESIAN_POINT('',(170.,-120.,20.));
#21594=CARTESIAN_POINT('',(-170.,-120.,20.));
#21595=CARTESIAN_POINT('',(170.,-120.,0.));
#21596=CARTESIAN_POINT('Origin',(170.,120.,0.));
#21597=CARTESIAN_POINT('',(170.,120.,0.));
#21598=CARTESIAN_POINT('',(170.,-120.,0.));
#21599=CARTESIAN_POINT('',(170.,120.,20.));
#21600=CARTESIAN_POINT('',(170.,-120.,20.));
#21601=CARTESIAN_POINT('',(170.,120.,0.));
#21602=CARTESIAN_POINT('Origin',(-170.,120.,0.));
#21603=CARTESIAN_POINT('',(-170.,120.,0.));
#21604=CARTESIAN_POINT('',(170.,120.,0.));
#21605=CARTESIAN_POINT('',(-170.,120.,20.));
#21606=CARTESIAN_POINT('',(170.,120.,20.));
#21607=CARTESIAN_POINT('',(-170.,120.,0.));
#21608=CARTESIAN_POINT('Origin',(-170.,-120.,0.));
#21609=CARTESIAN_POINT('',(-170.,120.,0.));
#21610=CARTESIAN_POINT('',(-170.,120.,20.));
#21611=CARTESIAN_POINT('Origin',(215.,155.,0.));
#21612=CARTESIAN_POINT('',(220.,155.,0.));
#21613=CARTESIAN_POINT('',(-220.,155.,0.));
#21614=CARTESIAN_POINT('',(107.5,155.,0.));
#21615=CARTESIAN_POINT('',(-220.,155.,20.));
#21616=CARTESIAN_POINT('',(-220.,155.,0.));
#21617=CARTESIAN_POINT('',(220.,155.,20.));
#21618=CARTESIAN_POINT('',(107.5,155.,20.));
#21619=CARTESIAN_POINT('',(220.,155.,0.));
#21620=CARTESIAN_POINT('Origin',(220.,-150.,0.));
#21621=CARTESIAN_POINT('',(220.,-155.,0.));
#21622=CARTESIAN_POINT('',(220.,-75.,0.));
#21623=CARTESIAN_POINT('',(220.,-155.,20.));
#21624=CARTESIAN_POINT('',(220.,-75.,20.));
#21625=CARTESIAN_POINT('',(220.,-155.,0.));
#21626=CARTESIAN_POINT('Origin',(-215.,-155.,0.));
#21627=CARTESIAN_POINT('',(-220.,-155.,0.));
#21628=CARTESIAN_POINT('',(-107.5,-155.,0.));
#21629=CARTESIAN_POINT('',(-220.,-155.,20.));
#21630=CARTESIAN_POINT('',(-107.5,-155.,20.));
#21631=CARTESIAN_POINT('',(-220.,-155.,0.));
#21632=CARTESIAN_POINT('Origin',(-220.,150.,0.));
#21633=CARTESIAN_POINT('',(-220.,75.,0.));
#21634=CARTESIAN_POINT('',(-220.,75.,20.));
#21635=CARTESIAN_POINT('Origin',(0.,0.,20.));
#21636=CARTESIAN_POINT('Origin',(0.,0.,0.));
#21637=CARTESIAN_POINT('',(0.,0.,0.));
#21638=CARTESIAN_POINT('Origin',(160.,0.,1.5));
#21639=CARTESIAN_POINT('',(155.5,5.51091059616309E-16,3.));
#21640=CARTESIAN_POINT('Origin',(160.,0.,3.));
#21641=CARTESIAN_POINT('',(155.5,5.51091059616309E-16,0.));
#21642=CARTESIAN_POINT('',(155.5,5.51091059616309E-16,1.5));
#21643=CARTESIAN_POINT('Origin',(160.,0.,0.));
#21644=CARTESIAN_POINT('Origin',(-160.,65.,1.5));
#21645=CARTESIAN_POINT('',(-163.5,65.,3.));
#21646=CARTESIAN_POINT('Origin',(-160.,65.,3.));
#21647=CARTESIAN_POINT('',(-163.5,65.,0.));
#21648=CARTESIAN_POINT('',(-163.5,65.,1.5));
#21649=CARTESIAN_POINT('Origin',(-160.,65.,0.));
#21650=CARTESIAN_POINT('Origin',(-160.,-95.,1.5));
#21651=CARTESIAN_POINT('',(-163.5,-95.,3.));
#21652=CARTESIAN_POINT('Origin',(-160.,-95.,3.));
#21653=CARTESIAN_POINT('',(-163.5,-95.,0.));
#21654=CARTESIAN_POINT('',(-163.5,-95.,1.5));
#21655=CARTESIAN_POINT('Origin',(-160.,-95.,0.));
#21656=CARTESIAN_POINT('Origin',(-160.,-65.,1.5));
#21657=CARTESIAN_POINT('',(-163.5,-65.,3.));
#21658=CARTESIAN_POINT('Origin',(-160.,-65.,3.));
#21659=CARTESIAN_POINT('',(-163.5,-65.,0.));
#21660=CARTESIAN_POINT('',(-163.5,-65.,1.5));
#21661=CARTESIAN_POINT('Origin',(-160.,-65.,0.));
#21662=CARTESIAN_POINT('Origin',(-160.,95.,1.5));
#21663=CARTESIAN_POINT('',(-163.5,95.,3.));
#21664=CARTESIAN_POINT('Origin',(-160.,95.,3.));
#21665=CARTESIAN_POINT('',(-163.5,95.,0.));
#21666=CARTESIAN_POINT('',(-163.5,95.,1.5));
#21667=CARTESIAN_POINT('Origin',(-160.,95.,0.));
#21668=CARTESIAN_POINT('Origin',(180.,130.,0.));
#21669=CARTESIAN_POINT('',(180.,130.,0.));
#21670=CARTESIAN_POINT('',(-180.,130.,0.));
#21671=CARTESIAN_POINT('',(180.,130.,0.));
#21672=CARTESIAN_POINT('',(-180.,130.,3.));
#21673=CARTESIAN_POINT('',(-180.,130.,0.));
#21674=CARTESIAN_POINT('',(180.,130.,3.));
#21675=CARTESIAN_POINT('',(180.,130.,3.));
#21676=CARTESIAN_POINT('',(180.,130.,0.));
#21677=CARTESIAN_POINT('Origin',(180.,-130.,0.));
#21678=CARTESIAN_POINT('',(180.,-130.,0.));
#21679=CARTESIAN_POINT('',(180.,-130.,0.));
#21680=CARTESIAN_POINT('',(180.,-130.,3.));
#21681=CARTESIAN_POINT('',(180.,-130.,3.));
#21682=CARTESIAN_POINT('',(180.,-130.,0.));
#21683=CARTESIAN_POINT('Origin',(-180.,-130.,0.));
#21684=CARTESIAN_POINT('',(-180.,-130.,0.));
#21685=CARTESIAN_POINT('',(-180.,-130.,0.));
#21686=CARTESIAN_POINT('',(-180.,-130.,3.));
#21687=CARTESIAN_POINT('',(-180.,-130.,3.));
#21688=CARTESIAN_POINT('',(-180.,-130.,0.));
#21689=CARTESIAN_POINT('Origin',(-180.,130.,0.));
#21690=CARTESIAN_POINT('',(-180.,130.,0.));
#21691=CARTESIAN_POINT('',(-180.,130.,3.));
#21692=CARTESIAN_POINT('Origin',(0.,0.,3.));
#21693=CARTESIAN_POINT('Origin',(0.,0.,0.));
#21694=CARTESIAN_POINT('',(0.,0.,0.));
#21695=CARTESIAN_POINT('Origin',(170.,-120.,0.));
#21696=CARTESIAN_POINT('',(170.,-120.,0.));
#21697=CARTESIAN_POINT('',(-170.,-120.,0.));
#21698=CARTESIAN_POINT('',(-170.,-120.,0.));
#21699=CARTESIAN_POINT('',(-170.,-120.,2.));
#21700=CARTESIAN_POINT('',(-170.,-120.,0.));
#21701=CARTESIAN_POINT('',(170.,-120.,2.));
#21702=CARTESIAN_POINT('',(-170.,-120.,2.));
#21703=CARTESIAN_POINT('',(170.,-120.,0.));
#21704=CARTESIAN_POINT('Origin',(170.,120.,0.));
#21705=CARTESIAN_POINT('',(170.,120.,0.));
#21706=CARTESIAN_POINT('',(170.,-120.,0.));
#21707=CARTESIAN_POINT('',(170.,120.,2.));
#21708=CARTESIAN_POINT('',(170.,-120.,2.));
#21709=CARTESIAN_POINT('',(170.,120.,0.));
#21710=CARTESIAN_POINT('Origin',(-170.,120.,0.));
#21711=CARTESIAN_POINT('',(-170.,120.,0.));
#21712=CARTESIAN_POINT('',(170.,120.,0.));
#21713=CARTESIAN_POINT('',(-170.,120.,2.));
#21714=CARTESIAN_POINT('',(170.,120.,2.));
#21715=CARTESIAN_POINT('',(-170.,120.,0.));
#21716=CARTESIAN_POINT('Origin',(-170.,-120.,0.));
#21717=CARTESIAN_POINT('',(-170.,120.,0.));
#21718=CARTESIAN_POINT('',(-170.,120.,2.));
#21719=CARTESIAN_POINT('Origin',(180.,130.,0.));
#21720=CARTESIAN_POINT('',(180.,130.,0.));
#21721=CARTESIAN_POINT('',(-180.,130.,0.));
#21722=CARTESIAN_POINT('',(180.,130.,0.));
#21723=CARTESIAN_POINT('',(-180.,130.,2.));
#21724=CARTESIAN_POINT('',(-180.,130.,0.));
#21725=CARTESIAN_POINT('',(180.,130.,2.));
#21726=CARTESIAN_POINT('',(180.,130.,2.));
#21727=CARTESIAN_POINT('',(180.,130.,0.));
#21728=CARTESIAN_POINT('Origin',(180.,-130.,0.));
#21729=CARTESIAN_POINT('',(180.,-130.,0.));
#21730=CARTESIAN_POINT('',(180.,-130.,0.));
#21731=CARTESIAN_POINT('',(180.,-130.,2.));
#21732=CARTESIAN_POINT('',(180.,-130.,2.));
#21733=CARTESIAN_POINT('',(180.,-130.,0.));
#21734=CARTESIAN_POINT('Origin',(-180.,-130.,0.));
#21735=CARTESIAN_POINT('',(-180.,-130.,0.));
#21736=CARTESIAN_POINT('',(-180.,-130.,0.));
#21737=CARTESIAN_POINT('',(-180.,-130.,2.));
#21738=CARTESIAN_POINT('',(-180.,-130.,2.));
#21739=CARTESIAN_POINT('',(-180.,-130.,0.));
#21740=CARTESIAN_POINT('Origin',(-180.,130.,0.));
#21741=CARTESIAN_POINT('',(-180.,130.,0.));
#21742=CARTESIAN_POINT('',(-180.,130.,2.));
#21743=CARTESIAN_POINT('Origin',(0.,0.,2.));
#21744=CARTESIAN_POINT('Origin',(0.,0.,0.));
#21745=CARTESIAN_POINT('',(0.,0.,0.));
#21746=CARTESIAN_POINT('Origin',(0.,0.,23.));
#21747=CARTESIAN_POINT('',(-1.66862128043148,-0.000391815337284296,18.7714803633902));
#21748=CARTESIAN_POINT('',(-1.66651971410499,0.00146964277546923,18.5785196366098));
#21749=CARTESIAN_POINT('',(-1.666,2.04026156737949E-16,23.));
#21750=CARTESIAN_POINT('',(-0.769902040670449,-1.47743251885542,18.));
#21751=CARTESIAN_POINT('Ctrl Pts',(-1.66651971410499,0.00146964277546923,
18.5785196366098));
#21752=CARTESIAN_POINT('Ctrl Pts',(-1.66756984451206,0.115275174909824,
18.5709016210591));
#21753=CARTESIAN_POINT('Ctrl Pts',(-1.65690316968289,0.228886355259084,
18.5632836055085));
#21754=CARTESIAN_POINT('Ctrl Pts',(-1.63379463140209,0.339911562034265,
18.5556655899578));
#21755=CARTESIAN_POINT('Ctrl Pts',(-1.52142398866744,0.87979745587462,18.5186212172939));
#21756=CARTESIAN_POINT('Ctrl Pts',(-1.1148509467417,1.35853498293726,18.4815768446301));
#21757=CARTESIAN_POINT('Ctrl Pts',(-0.600441280316438,1.55695868566131,
18.4445324719662));
#21758=CARTESIAN_POINT('Ctrl Pts',(-0.0860316138911562,1.75538238838537,
18.4074880993024));
#21759=CARTESIAN_POINT('Ctrl Pts',(0.536214677033665,1.67349226677081,18.3704437266385));
#21760=CARTESIAN_POINT('Ctrl Pts',(0.982144949096516,1.34892973433264,18.3333993539747));
#21761=CARTESIAN_POINT('Ctrl Pts',(1.42807522115936,1.02436720189448,18.2963549813108));
#21762=CARTESIAN_POINT('Ctrl Pts',(1.69768947436024,0.457132258632721,18.259310608647));
#21763=CARTESIAN_POINT('Ctrl Pts',(1.66642050747925,-0.0935369959750123,
18.2222662359831));
#21764=CARTESIAN_POINT('Ctrl Pts',(1.63515154059826,-0.644206250582737,
18.1852218633193));
#21765=CARTESIAN_POINT('Ctrl Pts',(1.30299935363541,-1.17830981653643,18.1481774906554));
#21766=CARTESIAN_POINT('Ctrl Pts',(0.824551049590138,-1.45061632146208,
18.1111331179916));
#21767=CARTESIAN_POINT('Ctrl Pts',(0.346102745544861,-1.72292282638774,
18.0740887453277));
#21768=CARTESIAN_POINT('Ctrl Pts',(-0.278641675582842,-1.73343227028534,
18.0370443726639));
#21769=CARTESIAN_POINT('Ctrl Pts',(-0.769902040670449,-1.47743251885542,
18.));
#21770=CARTESIAN_POINT('',(-1.33705952834865,0.998970281948476,18.));
#21771=CARTESIAN_POINT('Origin',(0.,0.,18.));
#21772=CARTESIAN_POINT('',(-1.66450505821393,-0.00123145023033004,18.0714803633902));
#21773=CARTESIAN_POINT('Ctrl Pts',(-1.33706021092905,0.998970828965241,
18.));
#21774=CARTESIAN_POINT('Ctrl Pts',(-1.54904561011422,0.714506920185143,
18.0238267877967));
#21775=CARTESIAN_POINT('Ctrl Pts',(-1.66218506517322,0.355909860131879,
18.0476535755935));
#21776=CARTESIAN_POINT('Ctrl Pts',(-1.66450505821393,-0.00123145023033004,
18.0714803633902));
#21777=CARTESIAN_POINT('',(-1.666,-2.04026156737949E-16,17.));
#21778=CARTESIAN_POINT('',(-1.666,2.04026156737949E-16,23.));
#21779=CARTESIAN_POINT('Origin',(0.,0.,17.));
#21780=CARTESIAN_POINT('Ctrl Pts',(-1.66450505821393,-0.00123145023033004,
18.0714803633902));
#21781=CARTESIAN_POINT('Ctrl Pts',(-1.66572133056423,-0.188465245039766,
18.0839717212025));
#21782=CARTESIAN_POINT('Ctrl Pts',(-1.63647939540381,-0.3752989338988,18.0964630790149));
#21783=CARTESIAN_POINT('Ctrl Pts',(-1.57505399404498,-0.550840946823039,
18.1089544368272));
#21784=CARTESIAN_POINT('Ctrl Pts',(-1.3928908142571,-1.0714283675521,18.1459988094911));
#21785=CARTESIAN_POINT('Ctrl Pts',(-0.927680991901669,-1.49270793428555,
18.1830431821549));
#21786=CARTESIAN_POINT('Ctrl Pts',(-0.391726107224654,-1.62209767954181,
18.2200875548188));
#21787=CARTESIAN_POINT('Ctrl Pts',(0.144228777452376,-1.75148742479807,
18.2571319274826));
#21788=CARTESIAN_POINT('Ctrl Pts',(0.750928724450993,-1.58898734857712,
18.2941763001465));
#21789=CARTESIAN_POINT('Ctrl Pts',(1.15043245240881,-1.20885486196241,18.3312206728103));
#21790=CARTESIAN_POINT('Ctrl Pts',(1.54993618036662,-0.828722375347701,
18.3682650454742));
#21791=CARTESIAN_POINT('Ctrl Pts',(1.74224368928364,-0.230957478339239,
18.405309418138));
#21792=CARTESIAN_POINT('Ctrl Pts',(1.63950887043352,0.31083583145342,18.4423537908019));
#21793=CARTESIAN_POINT('Ctrl Pts',(1.53677405158339,0.85262914124608,18.4793981634657));
#21794=CARTESIAN_POINT('Ctrl Pts',(1.13899690496613,1.33845086382294,18.5164425361296));
#21795=CARTESIAN_POINT('Ctrl Pts',(0.628126141256631,1.54600803039379,18.5534869087934));
#21796=CARTESIAN_POINT('Ctrl Pts',(0.117255377547129,1.75356519696465,18.5905312814573));
#21797=CARTESIAN_POINT('Ctrl Pts',(-0.506709003254616,1.6828578075295,18.6275756541212));
#21798=CARTESIAN_POINT('Ctrl Pts',(-0.958186006148353,1.36622807375104,
18.664620026785));
#21799=CARTESIAN_POINT('Ctrl Pts',(-1.39230488421667,1.06177193554254,18.7002401389867));
#21800=CARTESIAN_POINT('Ctrl Pts',(-1.66694480132652,0.52994008771394,18.7358602511885));
#21801=CARTESIAN_POINT('Ctrl Pts',(-1.66862128043148,-0.000391815337284296,
18.7714803633902));
#21802=CARTESIAN_POINT('Origin',(0.,0.,23.));
#21803=CARTESIAN_POINT('',(-1.66554933918236,0.00151251337263472,19.4714803633902));
#21804=CARTESIAN_POINT('',(-1.66327374781977,-4.03244713725982E-5,19.2785196366098));
#21805=CARTESIAN_POINT('',(-1.666,2.04026156737949E-16,23.));
#21806=CARTESIAN_POINT('Ctrl Pts',(-1.66327374781977,-4.03244713725982E-5,
19.2785196366098));
#21807=CARTESIAN_POINT('Ctrl Pts',(-1.66321388055115,0.280452962555568,
19.2598345237089));
#21808=CARTESIAN_POINT('Ctrl Pts',(-1.59604427325322,0.560973406431315,
19.241149410808));
#21809=CARTESIAN_POINT('Ctrl Pts',(-1.46192619363535,0.804645854884145,
19.2224642979072));
#21810=CARTESIAN_POINT('Ctrl Pts',(-1.19602894438243,1.28774130291723,19.1854199252433));
#21811=CARTESIAN_POINT('Ctrl Pts',(-0.666987552272445,1.62600395887066,
19.1483755525795));
#21812=CARTESIAN_POINT('Ctrl Pts',(-0.116907900542003,1.66463648121937,
19.1113311799156));
#21813=CARTESIAN_POINT('Ctrl Pts',(0.433171751188448,1.70326900356808,19.0742868072517));
#21814=CARTESIAN_POINT('Ctrl Pts',(1.00428966253935,1.44227139231205,19.0372424345879));
#21815=CARTESIAN_POINT('Ctrl Pts',(1.33510282367111,1.00108454580982,19.000198061924));
#21816=CARTESIAN_POINT('Ctrl Pts',(1.66591598480286,0.559897699307611,18.9631536892602));
#21817=CARTESIAN_POINT('Ctrl Pts',(1.75642439571548,-0.0614783824407909,
18.9261093165963));
#21818=CARTESIAN_POINT('Ctrl Pts',(1.56518696899417,-0.578696033473889,
18.8890649439325));
#21819=CARTESIAN_POINT('Ctrl Pts',(1.37394954227287,-1.09591368450699,18.8520205712686));
#21820=CARTESIAN_POINT('Ctrl Pts',(0.900966277917629,-1.5089729048248,18.8149761986048));
#21821=CARTESIAN_POINT('Ctrl Pts',(0.362727183275646,-1.62883763630031,
18.7779318259409));
#21822=CARTESIAN_POINT('Ctrl Pts',(-0.175511911366353,-1.74870236777582,
18.7408874532771));
#21823=CARTESIAN_POINT('Ctrl Pts',(-0.779006836295083,-1.57537261040905,
18.7038430806132));
#21824=CARTESIAN_POINT('Ctrl Pts',(-1.17167017698769,-1.18819060141662,
18.6667987079494));
#21825=CARTESIAN_POINT('Ctrl Pts',(-1.48358399432579,-0.880630903543001,
18.6373723508362));
#21826=CARTESIAN_POINT('Ctrl Pts',(-1.66246334113382,-0.438130697729091,
18.607945993723));
#21827=CARTESIAN_POINT('Ctrl Pts',(-1.66651971410499,0.00146964277546923,
18.5785196366098));
#21828=CARTESIAN_POINT('Ctrl Pts',(-1.66862128043148,-0.000391815337284296,
18.7714803633902));
#21829=CARTESIAN_POINT('Ctrl Pts',(-1.66868831399082,-0.0215969917005588,
18.7729046238523));
#21830=CARTESIAN_POINT('Ctrl Pts',(-1.6683189395033,-0.042799769984532,
18.7743288843144));
#21831=CARTESIAN_POINT('Ctrl Pts',(-1.66750590227882,-0.0639855189198817,
18.7757531447766));
#21832=CARTESIAN_POINT('Ctrl Pts',(-1.64635917052983,-0.615017299690576,
18.8127975174404));
#21833=CARTESIAN_POINT('Ctrl Pts',(-1.3250760820461,-1.15452878311018,18.8498418901043));
#21834=CARTESIAN_POINT('Ctrl Pts',(-0.850670573251791,-1.43563292242657,
18.8868862627681));
#21835=CARTESIAN_POINT('Ctrl Pts',(-0.376265064457497,-1.71673706174295,
18.923930635432));
#21836=CARTESIAN_POINT('Ctrl Pts',(0.251262864647364,-1.73943385695613,
18.9609750080958));
#21837=CARTESIAN_POINT('Ctrl Pts',(0.74473808845371,-1.49333471419146,18.9980193807597));
#21838=CARTESIAN_POINT('Ctrl Pts',(1.23821331226007,-1.24723557142679,19.0350637534235));
#21839=CARTESIAN_POINT('Ctrl Pts',(1.59763583076791,-0.732340490684249,
19.0721081260874));
#21840=CARTESIAN_POINT('Ctrl Pts',(1.6585299445115,-0.184276682906552,19.1091524987512));
#21841=CARTESIAN_POINT('Ctrl Pts',(1.71942405825509,0.363787124871138,19.1461968714151));
#21842=CARTESIAN_POINT('Ctrl Pts',(1.48178976723445,0.945019659683982,19.1832412440789));
#21843=CARTESIAN_POINT('Ctrl Pts',(1.05437157772921,1.29343804143271,19.2202856167428));
#21844=CARTESIAN_POINT('Ctrl Pts',(0.626953388223968,1.64185642318143,19.2573299894067));
#21845=CARTESIAN_POINT('Ctrl Pts',(0.00975130023412978,1.75746065186603,
19.2943743620705));
#21846=CARTESIAN_POINT('Ctrl Pts',(-0.514790020800312,1.58734766279481,
19.3314187347344));
#21847=CARTESIAN_POINT('Ctrl Pts',(-1.03933134183475,1.41723467372359,19.3684631073982));
#21848=CARTESIAN_POINT('Ctrl Pts',(-1.47121189591379,0.961404466896546,
19.4055074800621));
#21849=CARTESIAN_POINT('Ctrl Pts',(-1.61279508090511,0.428454068820398,
19.4425518527259));
#21850=CARTESIAN_POINT('Ctrl Pts',(-1.64964989746138,0.289724394418121,
19.452194689614));
#21851=CARTESIAN_POINT('Ctrl Pts',(-1.66683453773576,0.145769155066602,
19.4618375265021));
#21852=CARTESIAN_POINT('Ctrl Pts',(-1.66554933918236,0.00151251337263472,
19.4714803633902));
#21853=CARTESIAN_POINT('Origin',(0.,0.,23.));
#21854=CARTESIAN_POINT('',(-1.66342907320707,-0.00052814431987333,20.1714803633902));
#21855=CARTESIAN_POINT('',(-1.66660945832472,-0.0014645595731799,19.9785196366098));
#21856=CARTESIAN_POINT('',(-1.666,2.04026156737949E-16,23.));
#21857=CARTESIAN_POINT('Ctrl Pts',(-1.66660945832472,-0.0014645595731799,
19.9785196366098));
#21858=CARTESIAN_POINT('Ctrl Pts',(-1.66253083892564,0.442903547938621,
19.9487674263587));
#21859=CARTESIAN_POINT('Ctrl Pts',(-1.47929031344958,0.890241199679583,
19.9190152161076));
#21860=CARTESIAN_POINT('Ctrl Pts',(-1.16122364049601,1.19843253381782,19.8892630058565));
#21861=CARTESIAN_POINT('Ctrl Pts',(-0.765199941234552,1.58216048334607,
19.8522186331927));
#21862=CARTESIAN_POINT('Ctrl Pts',(-0.160159946883716,1.75017472804193,
19.8151742605288));
#21863=CARTESIAN_POINT('Ctrl Pts',(0.377018012610026,1.62558860949911,19.778129887865));
#21864=CARTESIAN_POINT('Ctrl Pts',(0.914195972103768,1.50100249095629,19.7410855152011));
#21865=CARTESIAN_POINT('Ctrl Pts',(1.38351189674041,1.08381600917481,19.7040411425372));
#21866=CARTESIAN_POINT('Ctrl Pts',(1.57019781685605,0.564941972855801,19.6669967698734));
#21867=CARTESIAN_POINT('Ctrl Pts',(1.75688373697169,0.0460679365367972,
19.6299523972095));
#21868=CARTESIAN_POINT('Ctrl Pts',(1.66093965256632,-0.574493654319738,
19.5929080245457));
#21869=CARTESIAN_POINT('Ctrl Pts',(1.32627101594693,-1.01276172717728,19.5558636518818));
#21870=CARTESIAN_POINT('Ctrl Pts',(0.991602379327531,-1.45102980003482,
19.518819279218));
#21871=CARTESIAN_POINT('Ctrl Pts',(0.418209190494114,-1.70700435489339,
19.4817749065541));
#21872=CARTESIAN_POINT('Ctrl Pts',(-0.131511680146043,-1.66354615959309,
19.4447305338903));
#21873=CARTESIAN_POINT('Ctrl Pts',(-0.681232550786199,-1.62008796429278,
19.4076861612264));
#21874=CARTESIAN_POINT('Ctrl Pts',(-1.20728110323309,-1.27719701883361,
19.3706417885626));
#21875=CARTESIAN_POINT('Ctrl Pts',(-1.46892882625861,-0.791787426047646,
19.3335974158987));
#21876=CARTESIAN_POINT('Ctrl Pts',(-1.59860192281783,-0.551217532038033,
19.3152381561358));
#21877=CARTESIAN_POINT('Ctrl Pts',(-1.66333257105202,-0.275642037215341,
19.2968788963728));
#21878=CARTESIAN_POINT('Ctrl Pts',(-1.66327374781977,-4.03244713725982E-5,
19.2785196366098));
#21879=CARTESIAN_POINT('Ctrl Pts',(-1.66554933918236,0.00151251337263472,
19.4714803633902));
#21880=CARTESIAN_POINT('Ctrl Pts',(-1.66189725893372,-0.408413898754999,
19.498881899166));
#21881=CARTESIAN_POINT('Ctrl Pts',(-1.50910204174448,-0.820774121553807,
19.5262834349417));
#21882=CARTESIAN_POINT('Ctrl Pts',(-1.23470683773252,-1.12257747109454,
19.5536849707175));
#21883=CARTESIAN_POINT('Ctrl Pts',(-0.863749593664997,-1.53058802360804,
19.5907293433813));
#21884=CARTESIAN_POINT('Ctrl Pts',(-0.27054928962637,-1.73653853930977,
19.6277737160452));
#21885=CARTESIAN_POINT('Ctrl Pts',(0.27343382250233,-1.64618196770234,19.664818088709));
#21886=CARTESIAN_POINT('Ctrl Pts',(0.817416934631023,-1.55582539609492,
19.7018624613729));
#21887=CARTESIAN_POINT('Ctrl Pts',(1.31218285484979,-1.16916173717834,19.7389068340367));
#21888=CARTESIAN_POINT('Ctrl Pts',(1.53131702289696,-0.663135912295698,
19.7759512067006));
#21889=CARTESIAN_POINT('Ctrl Pts',(1.75045119094414,-0.157110087413051,
19.8129955793645));
#21890=CARTESIAN_POINT('Ctrl Pts',(1.69395360681972,0.46827790343567,19.8500399520283));
#21891=CARTESIAN_POINT('Ctrl Pts',(1.38767864477499,0.92683821933391,19.8870843246922));
#21892=CARTESIAN_POINT('Ctrl Pts',(1.08140368273026,1.38539853523215,19.924128697356));
#21893=CARTESIAN_POINT('Ctrl Pts',(0.525351342765218,1.67713117617991,19.9611730700199));
#21894=CARTESIAN_POINT('Ctrl Pts',(-0.0260178646503011,1.66853353860585,
19.9982174426837));
#21895=CARTESIAN_POINT('Ctrl Pts',(-0.577387072065821,1.6599359010318,20.0352618153476));
#21896=CARTESIAN_POINT('Ctrl Pts',(-1.12407314693182,1.35100798493592,20.0723061880114));
#21897=CARTESIAN_POINT('Ctrl Pts',(-1.41590179139748,0.883121287398709,
20.1093505606753));
#21898=CARTESIAN_POINT('Ctrl Pts',(-1.5790507827593,0.621545721660193,20.1300604949136));
#21899=CARTESIAN_POINT('Ctrl Pts',(-1.66254528607668,0.31028833838162,20.1507704291519));
#21900=CARTESIAN_POINT('Ctrl Pts',(-1.66342907320707,-0.00052814431987333,
20.1714803633902));
#21901=CARTESIAN_POINT('Origin',(0.,0.,23.));
#21902=CARTESIAN_POINT('',(-1.6674840545265,-0.00123301224869695,20.8714803633902));
#21903=CARTESIAN_POINT('',(-1.66803766879579,0.000959062403117482,20.6785196366098));
#21904=CARTESIAN_POINT('',(-1.666,2.04026156737949E-16,23.));
#21905=CARTESIAN_POINT('Ctrl Pts',(-1.66803766879579,0.000959062403117482,
20.6785196366098));
#21906=CARTESIAN_POINT('Ctrl Pts',(-1.66842376314776,0.0572146414461489,
20.6747447016723));
#21907=CARTESIAN_POINT('Ctrl Pts',(-1.66582448293573,0.113434120530944,
20.6709697667349));
#21908=CARTESIAN_POINT('Ctrl Pts',(-1.66012222476806,0.169337087226355,
20.6671948317974));
#21909=CARTESIAN_POINT('Ctrl Pts',(-1.60416455130123,0.71792676243648,20.6301504591336));
#21910=CARTESIAN_POINT('Ctrl Pts',(-1.24939060962216,1.23603634645977,20.5931060864697));
#21911=CARTESIAN_POINT('Ctrl Pts',(-0.758151936074614,1.48656869769561,
20.5560617138059));
#21912=CARTESIAN_POINT('Ctrl Pts',(-0.266913262527071,1.73710104893144,
20.519017341142));
#21913=CARTESIAN_POINT('Ctrl Pts',(0.360790142888952,1.72005616737984,20.4819729684781));
#21914=CARTESIAN_POINT('Ctrl Pts',(0.837708846366109,1.44323412561422,20.4449285958143));
#21915=CARTESIAN_POINT('Ctrl Pts',(1.31462754984327,1.1664120838486,20.4078842231504));
#21916=CARTESIAN_POINT('Ctrl Pts',(1.64076155138155,0.629812881868986,20.3708398504866));
#21917=CARTESIAN_POINT('Ctrl Pts',(1.66686551824842,0.0789948759482206,
20.3337954778227));
#21918=CARTESIAN_POINT('Ctrl Pts',(1.69296948511529,-0.471823129972545,
20.2967511051589));
#21919=CARTESIAN_POINT('Ctrl Pts',(1.4190434173107,-1.03685993983447,20.259706732495));
#21920=CARTESIAN_POINT('Ctrl Pts',(0.970441265381544,-1.35754359208473,
20.2226623598312));
#21921=CARTESIAN_POINT('Ctrl Pts',(0.521839113452374,-1.67822724433501,
20.1856179871673));
#21922=CARTESIAN_POINT('Ctrl Pts',(-0.101439122601358,-1.75455773897363,
20.1485736145035));
#21923=CARTESIAN_POINT('Ctrl Pts',(-0.614169038869319,-1.55160473476285,
20.1115292418396));
#21924=CARTESIAN_POINT('Ctrl Pts',(-1.12689895513726,-1.34865173055207,
20.0744848691758));
#21925=CARTESIAN_POINT('Ctrl Pts',(-1.52908055161943,-0.866415227491897,
20.0374404965119));
#21926=CARTESIAN_POINT('Ctrl Pts',(-1.63666764777447,-0.325576148781487,
20.0003961238481));
#21927=CARTESIAN_POINT('Ctrl Pts',(-1.65784610275328,-0.219112302385464,
19.9931039614353));
#21928=CARTESIAN_POINT('Ctrl Pts',(-1.66760911363862,-0.1103776246422,19.9858117990225));
#21929=CARTESIAN_POINT('Ctrl Pts',(-1.66660945832472,-0.0014645595731799,
19.9785196366098));
#21930=CARTESIAN_POINT('Ctrl Pts',(-1.66342907320707,-0.00052814431987333,
20.1714803633902));
#21931=CARTESIAN_POINT('Ctrl Pts',(-1.66412613802131,-0.24567680775405,
20.1878148018158));
#21932=CARTESIAN_POINT('Ctrl Pts',(-1.61343216789926,-0.490551192765208,
20.2041492402413));
#21933=CARTESIAN_POINT('Ctrl Pts',(-1.50989667393363,-0.710558323734967,
20.2204836786668));
#21934=CARTESIAN_POINT('Ctrl Pts',(-1.2750916979388,-1.20950575835288,20.2575280513307));
#21935=CARTESIAN_POINT('Ctrl Pts',(-0.768510531883807,-1.58055514861014,
20.2945724239946));
#21936=CARTESIAN_POINT('Ctrl Pts',(-0.221974689125013,-1.65390699052376,
20.3316167966584));
#21937=CARTESIAN_POINT('Ctrl Pts',(0.324561153633781,-1.72725883243739,
20.3686611693222));
#21938=CARTESIAN_POINT('Ctrl Pts',(0.911051673096376,-1.50291312600738,
20.4057055419861));
#21939=CARTESIAN_POINT('Ctrl Pts',(1.26910726675768,-1.08353488200329,20.4427499146499));
#21940=CARTESIAN_POINT('Ctrl Pts',(1.62716286041898,-0.664156637999206,
20.4797942873138));
#21941=CARTESIAN_POINT('Ctrl Pts',(1.75678352827899,-0.0497458564210427,
20.5168386599777));
#21942=CARTESIAN_POINT('Ctrl Pts',(1.59865230117954,0.478530997816609,20.5538830326415));
#21943=CARTESIAN_POINT('Ctrl Pts',(1.44052107408009,1.00680785205427,20.5909274053054));
#21944=CARTESIAN_POINT('Ctrl Pts',(0.994637952021168,1.44895077895141,20.6279717779692));
#21945=CARTESIAN_POINT('Ctrl Pts',(0.46504782688183,1.60262647375647,20.6650161506331));
#21946=CARTESIAN_POINT('Ctrl Pts',(-0.0645422982574929,1.75630216856152,
20.7020605232969));
#21947=CARTESIAN_POINT('Ctrl Pts',(-0.677839426477227,1.62151063127449,
20.7391048959608));
#21948=CARTESIAN_POINT('Ctrl Pts',(-1.09418672250608,1.25993512208958,20.7761492686246));
#21949=CARTESIAN_POINT('Ctrl Pts',(-1.45133357711098,0.949772051404937,
20.8079263002132));
#21950=CARTESIAN_POINT('Ctrl Pts',(-1.6635572776099,0.472732735422094,20.8397033318017));
#21951=CARTESIAN_POINT('Ctrl Pts',(-1.6674840545265,-0.00123301224869695,
20.8714803633902));
#21952=CARTESIAN_POINT('Origin',(0.,0.,23.));
#21953=CARTESIAN_POINT('',(-1.66726411708323,0.00131035561855258,21.5714803633902));
#21954=CARTESIAN_POINT('',(-1.66370962959227,0.000855487351938633,21.3785196366098));
#21955=CARTESIAN_POINT('',(-1.666,2.04026156737949E-16,23.));
#21956=CARTESIAN_POINT('Ctrl Pts',(-1.66370962959227,0.000855487351938633,
21.3785196366098));
#21957=CARTESIAN_POINT('Ctrl Pts',(-1.66474566899998,0.223512053075316,
21.3636776043221));
#21958=CARTESIAN_POINT('Ctrl Pts',(-1.62319372826002,0.445797790127472,
21.3488355720344));
#21959=CARTESIAN_POINT('Ctrl Pts',(-1.53722532564539,0.649322068833036,
21.3339935397468));
#21960=CARTESIAN_POINT('Ctrl Pts',(-1.32265595387433,1.15730029448153,21.2969491670829));
#21961=CARTESIAN_POINT('Ctrl Pts',(-0.83139133092368,1.54840278958771,21.2599047944191));
#21962=CARTESIAN_POINT('Ctrl Pts',(-0.288243816224439,1.64365335557573,
21.2228604217552));
#21963=CARTESIAN_POINT('Ctrl Pts',(0.254903698474809,1.73890392156375,21.1858160490914));
#21964=CARTESIAN_POINT('Ctrl Pts',(0.849934104922654,1.53830255843362,21.1487716764275));
#21965=CARTESIAN_POINT('Ctrl Pts',(1.22454977899659,1.13364839773686,21.1117273037637));
#21966=CARTESIAN_POINT('Ctrl Pts',(1.59916545307052,0.728994237040111,21.0746829310998));
#21967=CARTESIAN_POINT('Ctrl Pts',(1.75336639477056,0.120287278776759,21.037638558436));
#21968=CARTESIAN_POINT('Ctrl Pts',(1.61658721862146,-0.413916193690381,
21.0005941857721));
#21969=CARTESIAN_POINT('Ctrl Pts',(1.47980804247235,-0.948119666157537,
20.9635498131082));
#21970=CARTESIAN_POINT('Ctrl Pts',(1.05204874847409,-1.40781965282848,20.9265054404444));
#21971=CARTESIAN_POINT('Ctrl Pts',(0.529060407604963,-1.58264839304365,
20.8894610677805));
#21972=CARTESIAN_POINT('Ctrl Pts',(0.00607206673584673,-1.75747713325882,
20.8524166951167));
#21973=CARTESIAN_POINT('Ctrl Pts',(-0.612145321004125,-1.64743462701824,
20.8153723224528));
#21974=CARTESIAN_POINT('Ctrl Pts',(-1.04268331224681,-1.30287849069947,
20.778327949789));
#21975=CARTESIAN_POINT('Ctrl Pts',(-1.42934816465156,-0.993433679080626,
20.7450585120626));
#21976=CARTESIAN_POINT('Ctrl Pts',(-1.66463492352674,-0.494835306173304,
20.7117890743362));
#21977=CARTESIAN_POINT('Ctrl Pts',(-1.66803766879579,0.000959062403117482,
20.6785196366098));
#21978=CARTESIAN_POINT('Ctrl Pts',(-1.6674840545265,-0.00123301224869695,
20.8714803633902));
#21979=CARTESIAN_POINT('Ctrl Pts',(-1.66813495463619,-0.0797972810366568,
20.8767477044655));
#21980=CARTESIAN_POINT('Ctrl Pts',(-1.6630626525888,-0.15827709993217,20.8820150455409));
#21981=CARTESIAN_POINT('Ctrl Pts',(-1.65197851677833,-0.235898443844886,
20.8872823866162));
#21982=CARTESIAN_POINT('Ctrl Pts',(-1.57402555118372,-0.78179701951157,
20.92432675928));
#21983=CARTESIAN_POINT('Ctrl Pts',(-1.19872215615655,-1.28523468976212,
20.9613711319439));
#21984=CARTESIAN_POINT('Ctrl Pts',(-0.697814551206597,-1.51582846911685,
20.9984155046078));
#21985=CARTESIAN_POINT('Ctrl Pts',(-0.196906946256626,-1.74642224847158,
21.0354598772716));
#21986=CARTESIAN_POINT('Ctrl Pts',(0.429604868616143,-1.70417213693048,
21.0725042499355));
#21987=CARTESIAN_POINT('Ctrl Pts',(0.895016757317744,-1.40841261701728,
21.1095486225993));
#21988=CARTESIAN_POINT('Ctrl Pts',(1.36042864601934,-1.11265309710409,21.1465929952632));
#21989=CARTESIAN_POINT('Ctrl Pts',(1.66474060854977,-0.563384168818808,
21.183637367927));
#21990=CARTESIAN_POINT('Ctrl Pts',(1.66869350204147,-0.0119621032475723,
21.2206817405909));
#21991=CARTESIAN_POINT('Ctrl Pts',(1.67264639553316,0.539459962323664,21.2577261132547));
#21992=CARTESIAN_POINT('Ctrl Pts',(1.37624021998613,1.09303516518086,21.2947704859186));
#21993=CARTESIAN_POINT('Ctrl Pts',(0.915116274553919,1.39543659824045,21.3318148585824));
#21994=CARTESIAN_POINT('Ctrl Pts',(0.453992329121703,1.69783803130004,21.3688592312463));
#21995=CARTESIAN_POINT('Ctrl Pts',(-0.171849386195692,1.74906569456202,
21.4059036039101));
#21996=CARTESIAN_POINT('Ctrl Pts',(-0.676011386027486,1.52567680116829,
21.442947976574));
#21997=CARTESIAN_POINT('Ctrl Pts',(-1.18017338585927,1.30228790777458,21.4799923492378));
#21998=CARTESIAN_POINT('Ctrl Pts',(-1.56265567020546,0.804282457725167,
21.5170367219017));
#21999=CARTESIAN_POINT('Ctrl Pts',(-1.64842681856946,0.259557545613813,
21.5540810945656));
#22000=CARTESIAN_POINT('Ctrl Pts',(-1.66185535629751,0.174274100385222,
21.5598808508404));
#22001=CARTESIAN_POINT('Ctrl Pts',(-1.668010973462,0.0878454775911748,21.5656806071153));
#22002=CARTESIAN_POINT('Ctrl Pts',(-1.66726411708323,0.00131035561855258,
21.5714803633902));
#22003=CARTESIAN_POINT('Origin',(0.,0.,23.));
#22004=CARTESIAN_POINT('',(-1.66336233325601,0.000403110553041652,22.2714803633902));
#22005=CARTESIAN_POINT('',(-1.66491696675796,-0.00142189824448361,22.0785196366098));
#22006=CARTESIAN_POINT('',(-1.666,2.04026156737949E-16,23.));
#22007=CARTESIAN_POINT('Ctrl Pts',(-1.66491696675796,-0.00142189824448361,
22.0785196366098));
#22008=CARTESIAN_POINT('Ctrl Pts',(-1.6617648131379,0.386551789612628,22.0526105069719));
#22009=CARTESIAN_POINT('Ctrl Pts',(-1.52658714042526,0.776505475615136,
22.026701377334));
#22010=CARTESIAN_POINT('Ctrl Pts',(-1.27881118667522,1.07206473672234,22.0007922476961));
#22011=CARTESIAN_POINT('Ctrl Pts',(-0.924545918171753,1.49464965430663,
21.9637478750323));
#22012=CARTESIAN_POINT('Ctrl Pts',(-0.340099051292463,1.72426662069324,
21.9267035023684));
#22013=CARTESIAN_POINT('Ctrl Pts',(0.207075025876924,1.65583839324593,21.8896591297046));
#22014=CARTESIAN_POINT('Ctrl Pts',(0.75424910304631,1.58741016579862,21.8526147570407));
#22015=CARTESIAN_POINT('Ctrl Pts',(1.26415039050579,1.22093674451738,21.8155703843769));
#22016=CARTESIAN_POINT('Ctrl Pts',(1.50343802435341,0.724123579106914,21.778526011713));
#22017=CARTESIAN_POINT('Ctrl Pts',(1.74272565820104,0.227310413696437,21.7414816390492));
#22018=CARTESIAN_POINT('Ctrl Pts',(1.7113996384368,-0.399842495843283,21.7044372663853));
#22019=CARTESIAN_POINT('Ctrl Pts',(1.42379536819668,-0.870337635857372,
21.6673928937215));
#22020=CARTESIAN_POINT('Ctrl Pts',(1.13619109795657,-1.34083277587145,21.6303485210576));
#22021=CARTESIAN_POINT('Ctrl Pts',(0.592308577240593,-1.65467014635991,
21.5933041483937));
#22022=CARTESIAN_POINT('Ctrl Pts',(0.0410391510285976,-1.66823159032892,
21.5562597757299));
#22023=CARTESIAN_POINT('Ctrl Pts',(-0.510230275183399,-1.68179303429794,
21.519215403066));
#22024=CARTESIAN_POINT('Ctrl Pts',(-1.06888660689141,-1.3950785517475,21.4821710304022));
#22025=CARTESIAN_POINT('Ctrl Pts',(-1.37927771244968,-0.939294332376885,
21.4451266577383));
#22026=CARTESIAN_POINT('Ctrl Pts',(-1.5653089090872,-0.666122575133674,
21.4229243173622));
#22027=CARTESIAN_POINT('Ctrl Pts',(-1.6621598081711,-0.332218633722869,
21.400721976986));
#22028=CARTESIAN_POINT('Ctrl Pts',(-1.66370962959227,0.000855487351938633,
21.3785196366098));
#22029=CARTESIAN_POINT('Ctrl Pts',(-1.66726411708323,0.00131035561855258,
21.5714803633902));
#22030=CARTESIAN_POINT('Ctrl Pts',(-1.66324063058717,-0.46487418077553,
21.6027249797792));
#22031=CARTESIAN_POINT('Ctrl Pts',(-1.45889191058994,-0.93414956173162,
21.6339695961681));
#22032=CARTESIAN_POINT('Ctrl Pts',(-1.11213714530839,-1.2441189917722,21.6652142125571));
#22033=CARTESIAN_POINT('Ctrl Pts',(-0.701016311301517,-1.61162624287356,
21.7022585852209));
#22034=CARTESIAN_POINT('Ctrl Pts',(-0.0897146309059634,-1.75519637090299,
21.7393029578848));
#22035=CARTESIAN_POINT('Ctrl Pts',(0.442024216629908,-1.60912885984179,
21.7763473305487));
#22036=CARTESIAN_POINT('Ctrl Pts',(0.973763064165779,-1.46306134878059,
21.8133917032125));
#22037=CARTESIAN_POINT('Ctrl Pts',(1.42593907884196,-1.02735619862877,21.8504360758764));
#22038=CARTESIAN_POINT('Ctrl Pts',(1.59162761760514,-0.501400660689515,
21.8874804485402));
#22039=CARTESIAN_POINT('Ctrl Pts',(1.75731615636832,0.02455487724974,21.9245248212041));
#22040=CARTESIAN_POINT('Ctrl Pts',(1.63651721921848,0.64076080297644,21.9615691938679));
#22041=CARTESIAN_POINT('Ctrl Pts',(1.28451077709545,1.06522915806354,21.9986135665318));
#22042=CARTESIAN_POINT('Ctrl Pts',(0.93250433497242,1.48969751315065,22.0356579391956));
#22043=CARTESIAN_POINT('Ctrl Pts',(0.34929038787619,1.72242829759816,22.0727023118595));
#22044=CARTESIAN_POINT('Ctrl Pts',(-0.19824088446344,1.65691932434573,22.1097466845233));
#22045=CARTESIAN_POINT('Ctrl Pts',(-0.745772156803077,1.59141035109329,
22.1467910571872));
#22046=CARTESIAN_POINT('Ctrl Pts',(-1.25762075438611,1.22766162014088,22.183835429851));
#22047=CARTESIAN_POINT('Ctrl Pts',(-1.49955468587626,0.732131709277595,
22.2208798025149));
#22048=CARTESIAN_POINT('Ctrl Pts',(-1.60971080179752,0.506509573650329,
22.23774665614));
#22049=CARTESIAN_POINT('Ctrl Pts',(-1.66391046875662,0.253567667020629,
22.2546135097651));
#22050=CARTESIAN_POINT('Ctrl Pts',(-1.66336233325601,0.000403110553041652,
22.2714803633902));
#22051=CARTESIAN_POINT('Origin',(0.,0.,23.));
#22052=CARTESIAN_POINT('',(-1.66578620297286,-0.00152257679421897,22.9714803633902));
#22053=CARTESIAN_POINT('',(-1.66873613391169,-1.89540107977907E-5,22.7785196366098));
#22054=CARTESIAN_POINT('',(-1.666,2.04026156737949E-16,23.));
#22055=CARTESIAN_POINT('Ctrl Pts',(-1.66873602989402,-1.89532902365601E-5,
22.7785196366098));
#22056=CARTESIAN_POINT('Ctrl Pts',(-1.66864347242946,0.550403095397029,
22.7415434096217));
#22057=CARTESIAN_POINT('Ctrl Pts',(-1.36953979702872,1.10091133072281,22.7045671826336));
#22058=CARTESIAN_POINT('Ctrl Pts',(-0.907660834486349,1.40029734714771,
22.6675909556455));
#22059=CARTESIAN_POINT('Ctrl Pts',(-0.444930647885177,1.70023511977004,
22.6305465829816));
#22060=CARTESIAN_POINT('Ctrl Pts',(0.181175355132312,1.74812420457462,22.5935022103178));
#22061=CARTESIAN_POINT('Ctrl Pts',(0.684138745939249,1.52204961390686,22.5564578376539));
#22062=CARTESIAN_POINT('Ctrl Pts',(1.1871021367462,1.2959750232391,22.51941346499));
#22063=CARTESIAN_POINT('Ctrl Pts',(1.56692291534261,0.795936757098989,22.4823690923262));
#22064=CARTESIAN_POINT('Ctrl Pts',(1.64978761864264,0.250762166729425,22.4453247196624));
#22065=CARTESIAN_POINT('Ctrl Pts',(1.73265232194267,-0.294412423640124,
22.4082803469985));
#22066=CARTESIAN_POINT('Ctrl Pts',(1.51856094994635,-0.88472333823912,22.3712359743346));
#22067=CARTESIAN_POINT('Ctrl Pts',(1.10548592775637,-1.25003268534147,22.3341916016708));
#22068=CARTESIAN_POINT('Ctrl Pts',(0.692410905566374,-1.61534203244382,
22.2971472290069));
#22069=CARTESIAN_POINT('Ctrl Pts',(0.0803522331827074,-1.75564981204952,
22.2601028563431));
#22070=CARTESIAN_POINT('Ctrl Pts',(-0.450599995714626,-1.60674842298081,
22.2230584836792));
#22071=CARTESIAN_POINT('Ctrl Pts',(-0.981552224611956,-1.4578470339121,
22.1860141110154));
#22072=CARTESIAN_POINT('Ctrl Pts',(-1.43139801002296,-1.01973647616899,
22.1489697383515));
#22073=CARTESIAN_POINT('Ctrl Pts',(-1.59427906766464,-0.492904762906453,
22.1119253656877));
#22074=CARTESIAN_POINT('Ctrl Pts',(-1.64323981475635,-0.334543350926403,
22.1007901226617));
#22075=CARTESIAN_POINT('Ctrl Pts',(-1.66627170144435,-0.168165488721959,
22.0896548796358));
#22076=CARTESIAN_POINT('Ctrl Pts',(-1.66491696675796,-0.00142189824448361,
22.0785196366098));
#22077=CARTESIAN_POINT('Ctrl Pts',(-1.66336233325601,0.000403110553041652,
22.2714803633902));
#22078=CARTESIAN_POINT('Ctrl Pts',(-1.66270660843943,-0.302453176197396,
22.291657882429));
#22079=CARTESIAN_POINT('Ctrl Pts',(-1.58370177298327,-0.605628095221617,
22.3118354014677));
#22080=CARTESIAN_POINT('Ctrl Pts',(-1.42841701687781,-0.862731662544646,
22.3320129205065));
#22081=CARTESIAN_POINT('Ctrl Pts',(-1.14332615099193,-1.33475403272947,
22.3690572931703));
#22082=CARTESIAN_POINT('Ctrl Pts',(-0.601125153822886,-1.65148768232495,
22.4061016658342));
#22083=CARTESIAN_POINT('Ctrl Pts',(-0.0499358720868693,-1.6679890600187,
22.443146038498));
#22084=CARTESIAN_POINT('Ctrl Pts',(0.501253409649147,-1.68449043771246,
22.4801904111619));
#22085=CARTESIAN_POINT('Ctrl Pts',(1.06143097595213,-1.4007595435045,22.5172347838257));
#22086=CARTESIAN_POINT('Ctrl Pts',(1.37424854829476,-0.946637218353961,
22.5542791564896));
#22087=CARTESIAN_POINT('Ctrl Pts',(1.68706612063737,-0.492514893203437,
22.5913235291534));
#22088=CARTESIAN_POINT('Ctrl Pts',(1.75252369901963,0.131998862889646,22.6283679018173));
#22089=CARTESIAN_POINT('Ctrl Pts',(1.54066660738123,0.641114264826145,22.6654122744811));
#22090=CARTESIAN_POINT('Ctrl Pts',(1.32880951574283,1.15022966676265,22.702456647145));
#22091=CARTESIAN_POINT('Ctrl Pts',(0.839637754083762,1.54394671454257,22.7395010198089));
#22092=CARTESIAN_POINT('Ctrl Pts',(0.297005947345673,1.64209273882581,22.7765453924727));
#22093=CARTESIAN_POINT('Ctrl Pts',(-0.245625859392417,1.74023876310906,
22.8135897651366));
#22094=CARTESIAN_POINT('Ctrl Pts',(-0.841717711209527,1.54281376389563,
22.8506341378004));
#22095=CARTESIAN_POINT('Ctrl Pts',(-1.21848624574082,1.14016330611172,22.8876785104643));
#22096=CARTESIAN_POINT('Ctrl Pts',(-1.50259508645847,0.836537752779009,
22.9156124614396));
#22097=CARTESIAN_POINT('Ctrl Pts',(-1.66199284431962,0.416217406185016,
22.9435464124149));
#22098=CARTESIAN_POINT('Ctrl Pts',(-1.66578620297286,-0.00152257679421897,
22.9714803633902));
#22099=CARTESIAN_POINT('Origin',(0.,0.,23.));
#22100=CARTESIAN_POINT('',(-1.66853019577507,0.000530614451512978,23.6714803633902));
#22101=CARTESIAN_POINT('',(-1.66497222359982,0.00143386426241622,23.4785196366098));
#22102=CARTESIAN_POINT('',(-1.666,2.04026156737949E-16,23.));
#22103=CARTESIAN_POINT('Ctrl Pts',(-1.66497222359982,0.00143386426241622,
23.4785196366098));
#22104=CARTESIAN_POINT('Ctrl Pts',(-1.66632491173626,0.16612274283444,23.4675206849353));
#22105=CARTESIAN_POINT('Ctrl Pts',(-1.64386439031773,0.330450820220333,
23.4565217332608));
#22106=CARTESIAN_POINT('Ctrl Pts',(-1.59607730938674,0.487050380710409,
23.4455227815864));
#22107=CARTESIAN_POINT('Ctrl Pts',(-1.4351308404033,1.01447632542622,23.4084784089225));
#22108=CARTESIAN_POINT('Ctrl Pts',(-0.986895966349284,1.45423488320508,
23.3714340362587));
#22109=CARTESIAN_POINT('Ctrl Pts',(-0.45649378676817,1.60508388364329,23.3343896635948));
#22110=CARTESIAN_POINT('Ctrl Pts',(0.073908392812964,1.75593288408151,23.297345290931));
#22111=CARTESIAN_POINT('Ctrl Pts',(0.686477877921196,1.61787232717907,23.2603009182671));
#22112=CARTESIAN_POINT('Ctrl Pts',(1.10089081692101,1.25408144077981,23.2232565456033));
#22113=CARTESIAN_POINT('Ctrl Pts',(1.51530375592082,0.890290554380557,23.1862121729394));
#22114=CARTESIAN_POINT('Ctrl Pts',(1.73156014881221,0.300769338484503,23.1491678002756));
#22115=CARTESIAN_POINT('Ctrl Pts',(1.65069681432376,-0.244705696849849,
23.1121234276117));
#22116=CARTESIAN_POINT('Ctrl Pts',(1.5698334798353,-0.790180732184218,23.0750790549479));
#22117=CARTESIAN_POINT('Ctrl Pts',(1.19185041796697,-1.29160958695689,23.038034682284));
#22118=CARTESIAN_POINT('Ctrl Pts',(0.689720116463903,-1.51952854920018,
23.0009903096202));
#22119=CARTESIAN_POINT('Ctrl Pts',(0.187589814960836,-1.74744751144346,
22.9639459369563));
#22120=CARTESIAN_POINT('Ctrl Pts',(-0.438687726176967,-1.70185658115737,
22.9269015642925));
#22121=CARTESIAN_POINT('Ctrl Pts',(-0.902515579102954,-1.40361906526159,
22.8898571916286));
#22122=CARTESIAN_POINT('Ctrl Pts',(-1.36719667532058,-1.10483292090776,
22.852744673289));
#22123=CARTESIAN_POINT('Ctrl Pts',(-1.66882892851784,-0.552469812676142,
22.8156321549494));
#22124=CARTESIAN_POINT('Ctrl Pts',(-1.66873602989402,-1.89532902365601E-5,
22.7785196366098));
#22125=CARTESIAN_POINT('Ctrl Pts',(-1.66578620297286,-0.00152257679421897,
22.9714803633902));
#22126=CARTESIAN_POINT('Ctrl Pts',(-1.66702337479211,-0.137764936654608,
22.9805907850788));
#22127=CARTESIAN_POINT('Ctrl Pts',(-1.6517091709214,-0.273732827619376,
22.9897012067673));
#22128=CARTESIAN_POINT('Ctrl Pts',(-1.61877186757403,-0.405288460746241,
22.9988116284558));
#22129=CARTESIAN_POINT('Ctrl Pts',(-1.48484373763047,-0.9402138534659,23.0358560011197));
#22130=CARTESIAN_POINT('Ctrl Pts',(-1.05954226049788,-1.40218872255081,
23.0729003737835));
#22131=CARTESIAN_POINT('Ctrl Pts',(-0.537493761963633,-1.57980427633088,
23.1099447464474));
#22132=CARTESIAN_POINT('Ctrl Pts',(-0.0154452634293974,-1.75741983011095,
23.1469891191112));
#22133=CARTESIAN_POINT('Ctrl Pts',(0.603350256506486,-1.65067606858619,
23.1840334917751));
#22134=CARTESIAN_POINT('Ctrl Pts',(1.03571979014419,-1.30842103772709,23.2210778644389));
#22135=CARTESIAN_POINT('Ctrl Pts',(1.46808932378189,-0.966166006867992,
23.2581222371028));
#22136=CARTESIAN_POINT('Ctrl Pts',(1.71403287112142,-0.388399706674552,
23.2951666097666));
#22137=CARTESIAN_POINT('Ctrl Pts',(1.66100182477836,0.160480633554725,23.3322109824305));
#22138=CARTESIAN_POINT('Ctrl Pts',(1.6079707784353,0.709360973784014,23.3692553550943));
#22139=CARTESIAN_POINT('Ctrl Pts',(1.25596513840964,1.22935535404913,23.4062997277582));
#22140=CARTESIAN_POINT('Ctrl Pts',(0.766069612980623,1.48250411255109,23.4433441004221));
#22141=CARTESIAN_POINT('Ctrl Pts',(0.276174087551608,1.73565287105304,23.4803884730859));
#22142=CARTESIAN_POINT('Ctrl Pts',(-0.351611323280771,1.72195600779182,
23.5174328457498));
#22143=CARTESIAN_POINT('Ctrl Pts',(-0.82999966082312,1.44768147694742,23.5544772184136));
#22144=CARTESIAN_POINT('Ctrl Pts',(-1.30838799836547,1.17340694610302,23.5915215910775));
#22145=CARTESIAN_POINT('Ctrl Pts',(-1.63737926261779,0.638554747675423,
23.6285659637413));
#22146=CARTESIAN_POINT('Ctrl Pts',(-1.66642057657324,0.0878837734537999,
23.6656103364052));
#22147=CARTESIAN_POINT('Ctrl Pts',(-1.66795453242439,0.0587974530393284,
23.6675670120668));
#22148=CARTESIAN_POINT('Ctrl Pts',(-1.6686516491224,0.0296669993588705,
23.6695236877285));
#22149=CARTESIAN_POINT('Ctrl Pts',(-1.66853019577507,0.000530614451512978,
23.6714803633902));
#22150=CARTESIAN_POINT('Origin',(0.,0.,23.));
#22151=CARTESIAN_POINT('',(-1.66422209409782,0.00118661478516524,24.3714803633902));
#22152=CARTESIAN_POINT('',(-1.66367848409818,-0.000827345116924024,24.1785196366098));
#22153=CARTESIAN_POINT('',(-1.666,2.04026156737949E-16,23.));
#22154=CARTESIAN_POINT('Ctrl Pts',(-1.66367848409818,-0.000827345116924024,
24.1785196366098));
#22155=CARTESIAN_POINT('Ctrl Pts',(-1.66219049440645,0.330217676389022,
24.1564535875851));
#22156=CARTESIAN_POINT('Ctrl Pts',(-1.56660725193993,0.662054420660071,
24.1343875385604));
#22157=CARTESIAN_POINT('Ctrl Pts',(-1.38271566821857,0.93422600678436,24.1123214895358));
#22158=CARTESIAN_POINT('Ctrl Pts',(-1.0739993978296,1.3911463033731,24.0752771168719));
#22159=CARTESIAN_POINT('Ctrl Pts',(-0.516399081127575,1.67990914425084,
24.0382327442081));
#22160=CARTESIAN_POINT('Ctrl Pts',(0.0349164034973534,1.66837097063458,
24.0011883715442));
#22161=CARTESIAN_POINT('Ctrl Pts',(0.586231888122278,1.65683279701833,23.9641439988803));
#22162=CARTESIAN_POINT('Ctrl Pts',(1.13126254067011,1.34499360890808,23.9270996262165));
#22163=CARTESIAN_POINT('Ctrl Pts',(1.42059160843624,0.875557155718521,23.8900552535526));
#22164=CARTESIAN_POINT('Ctrl Pts',(1.70992067620237,0.406120702528958,23.8530108808888));
#22165=CARTESIAN_POINT('Ctrl Pts',(1.7435481591868,-0.220913015739925,23.8159665082249));
#22166=CARTESIAN_POINT('Ctrl Pts',(1.50608545939344,-0.718601029704961,
23.7789221355611));
#22167=CARTESIAN_POINT('Ctrl Pts',(1.26862275960007,-1.21628904367,23.7418777628972));
#22168=CARTESIAN_POINT('Ctrl Pts',(0.760069877028919,-1.58463135333119,
23.7048333902334));
#22169=CARTESIAN_POINT('Ctrl Pts',(0.213150618967734,-1.65506726888155,
23.6677890175695));
#22170=CARTESIAN_POINT('Ctrl Pts',(-0.333768639093451,-1.72550318443192,
23.6307446449057));
#22171=CARTESIAN_POINT('Ctrl Pts',(-0.919054272644665,-1.49803270587146,
23.5937002722418));
#22172=CARTESIAN_POINT('Ctrl Pts',(-1.27486805746385,-1.07675080076484,
23.556655899578));
#22173=CARTESIAN_POINT('Ctrl Pts',(-1.52503614381627,-0.780552922796213,
23.5306104785886));
#22174=CARTESIAN_POINT('Ctrl Pts',(-1.66176906996994,-0.388547954153529,
23.5045650575992));
#22175=CARTESIAN_POINT('Ctrl Pts',(-1.66497222359982,0.00143386426241622,
23.4785196366098));
#22176=CARTESIAN_POINT('Ctrl Pts',(-1.66853019577507,0.000530614451512978,
23.6714803633902));
#22177=CARTESIAN_POINT('Ctrl Pts',(-1.66635225778858,-0.521951810913478,
23.7065680603924));
#22178=CARTESIAN_POINT('Ctrl Pts',(-1.40094886176378,-1.04634152561339,
23.7416557573946));
#22179=CARTESIAN_POINT('Ctrl Pts',(-0.977667790968778,-1.35234861857636,
23.7767434543967));
#22180=CARTESIAN_POINT('Ctrl Pts',(-0.530782327750313,-1.67542028636924,
23.8137878270606));
#22181=CARTESIAN_POINT('Ctrl Pts',(0.0920799623451787,-1.75507387193934,
23.8508321997244));
#22182=CARTESIAN_POINT('Ctrl Pts',(0.605885037559579,-1.55485832696249,
23.8878765723883));
#22183=CARTESIAN_POINT('Ctrl Pts',(1.11969011277398,-1.35464278198564,23.9249209450521));
#22184=CARTESIAN_POINT('Ctrl Pts',(1.52443797310729,-0.874558106461856,
23.961965317716));
#22185=CARTESIAN_POINT('Ctrl Pts',(1.63490803231072,-0.334300495885159,
23.9990096903798));
#22186=CARTESIAN_POINT('Ctrl Pts',(1.74537809151414,0.205957114691539,24.0360540630437));
#22187=CARTESIAN_POINT('Ctrl Pts',(1.56157034958768,0.806387660321145,24.0730984357075));
#22188=CARTESIAN_POINT('Ctrl Pts',(1.167598846538,1.19222230696557,24.1101428083714));
#22189=CARTESIAN_POINT('Ctrl Pts',(0.773627343488314,1.57805695360998,24.1471871810353));
#22190=CARTESIAN_POINT('Ctrl Pts',(0.169492079315405,1.74929570126922,24.1842315536991));
#22191=CARTESIAN_POINT('Ctrl Pts',(-0.368342759829064,1.62757632906868,
24.221275926363));
#22192=CARTESIAN_POINT('Ctrl Pts',(-0.906177598973534,1.50585695686814,
24.2583202990268));
#22193=CARTESIAN_POINT('Ctrl Pts',(-1.37771201308956,1.09117946480783,24.2953646716907));
#22194=CARTESIAN_POINT('Ctrl Pts',(-1.56716257457082,0.573308434028074,
24.3324090443545));
#22195=CARTESIAN_POINT('Ctrl Pts',(-1.63376813250798,0.39123935661342,24.3454328173664));
#22196=CARTESIAN_POINT('Ctrl Pts',(-1.66550726908954,0.196415244238198,
24.3584565903783));
#22197=CARTESIAN_POINT('Ctrl Pts',(-1.66422209409782,0.00118661478516524,
24.3714803633902));
#22198=CARTESIAN_POINT('Origin',(0.,0.,23.));
#22199=CARTESIAN_POINT('',(-1.66424525785499,-0.00119753195345899,25.0714803633902));
#22200=CARTESIAN_POINT('',(-1.66799179081971,-0.000987328612398951,24.8785196366098));
#22201=CARTESIAN_POINT('',(-1.666,2.04026156737949E-16,23.));
#22202=CARTESIAN_POINT('Ctrl Pts',(-1.66799179081971,-0.000987328612398951,
24.8785196366098));
#22203=CARTESIAN_POINT('Ctrl Pts',(-1.66452448203087,0.492811694213693,
24.8453864902349));
#22204=CARTESIAN_POINT('Ctrl Pts',(-1.43140513105353,0.989454702814845,
24.81225334386));
#22205=CARTESIAN_POINT('Ctrl Pts',(-1.04745790195205,1.29904303028329,24.7791201974851));
#22206=CARTESIAN_POINT('Ctrl Pts',(-0.618187343787852,1.64517693635291,
24.7420758248212));
#22207=CARTESIAN_POINT('Ctrl Pts',(-0.000377979727074346,1.75748758204953,
24.7050314521574));
#22208=CARTESIAN_POINT('Ctrl Pts',(0.523248466866253,1.58457940565043,24.6679870794936));
#22209=CARTESIAN_POINT('Ctrl Pts',(1.04687491345958,1.41167122925133,24.6309427068297));
#22210=CARTESIAN_POINT('Ctrl Pts',(1.47631844258546,0.953544230756513,24.5938983341658));
#22211=CARTESIAN_POINT('Ctrl Pts',(1.61505724394959,0.419846340528664,24.556853961502));
#22212=CARTESIAN_POINT('Ctrl Pts',(1.75379604531373,-0.113851549699185,
24.5198095888381));
#22213=CARTESIAN_POINT('Ctrl Pts',(1.60183011891612,-0.72312033166006,24.4827652161743));
#22214=CARTESIAN_POINT('Ctrl Pts',(1.2287020633366,-1.12914662043587,24.4457208435104));
#22215=CARTESIAN_POINT('Ctrl Pts',(0.855574007757078,-1.53517290921169,
24.4086764708466));
#22216=CARTESIAN_POINT('Ctrl Pts',(0.261283822995645,-1.73795670480244,
24.3716320981827));
#22217=CARTESIAN_POINT('Ctrl Pts',(-0.282209606884,-1.6447001515996,24.3345877255189));
#22218=CARTESIAN_POINT('Ctrl Pts',(-0.825703036763652,-1.55144359839676,
24.297543352855));
#22219=CARTESIAN_POINT('Ctrl Pts',(-1.31839971176152,-1.16214669640031,
24.2604989801912));
#22220=CARTESIAN_POINT('Ctrl Pts',(-1.53483193722248,-0.654959369252205,
24.2234546075273));
#22221=CARTESIAN_POINT('Ctrl Pts',(-1.622342986426,-0.449885956330785,24.2084762838881));
#22222=CARTESIAN_POINT('Ctrl Pts',(-1.66468852405365,-0.22553904886167,
24.193497960249));
#22223=CARTESIAN_POINT('Ctrl Pts',(-1.66367848409818,-0.000827345116924024,
24.1785196366098));
#22224=CARTESIAN_POINT('Ctrl Pts',(-1.66422209409782,0.00118661478516524,
24.3714803633902));
#22225=CARTESIAN_POINT('Ctrl Pts',(-1.6618517614814,-0.35888636440512,24.3955009630422));
#22226=CARTESIAN_POINT('Ctrl Pts',(-1.54714313437419,-0.720335383138663,
24.4195215626941));
#22227=CARTESIAN_POINT('Ctrl Pts',(-1.3316535181475,-1.0056739050351,24.4435421623461));
#22228=CARTESIAN_POINT('Ctrl Pts',(-0.999327191396451,-1.4457206438193,
24.4805865350099));
#22229=CARTESIAN_POINT('Ctrl Pts',(-0.427307829047882,-1.7047495518885,
24.5176309076738));
#22230=CARTESIAN_POINT('Ctrl Pts',(0.122637251456149,-1.66422390327097,
24.5546752803376));
#22231=CARTESIAN_POINT('Ctrl Pts',(0.672582331960171,-1.62369825465344,
24.5917196530015));
#22232=CARTESIAN_POINT('Ctrl Pts',(1.20045313061966,-1.28361804934919,24.6287640256653));
#22233=CARTESIAN_POINT('Ctrl Pts',(1.46468558157194,-0.799610682018708,
24.6658083983292));
#22234=CARTESIAN_POINT('Ctrl Pts',(1.72891803252422,-0.315603314688219,
24.702852770993));
#22235=CARTESIAN_POINT('Ctrl Pts',(1.7295121357693,0.31233121466851,24.7398971436569));
#22236=CARTESIAN_POINT('Ctrl Pts',(1.46619601797039,0.796837707786795,24.7769415163208));
#22237=CARTESIAN_POINT('Ctrl Pts',(1.20287990017147,1.28134420090509,24.8139858889846));
#22238=CARTESIAN_POINT('Ctrl Pts',(0.675653561328557,1.62242265778493,24.8510302616485));
#22239=CARTESIAN_POINT('Ctrl Pts',(0.125786149809405,1.66398886419934,24.8880746343123));
#22240=CARTESIAN_POINT('Ctrl Pts',(-0.424081261709735,1.70555507061376,
24.9251190069762));
#22241=CARTESIAN_POINT('Ctrl Pts',(-0.996589745905115,1.44760902656276,
24.96216337964));
#22242=CARTESIAN_POINT('Ctrl Pts',(-1.32974815355174,1.00819191813303,24.9992077523039));
#22243=CARTESIAN_POINT('Ctrl Pts',(-1.54640929346339,0.722428121020488,
25.023298622666));
#22244=CARTESIAN_POINT('Ctrl Pts',(-1.6618439702268,0.35991618045346,25.0473894930281));
#22245=CARTESIAN_POINT('Ctrl Pts',(-1.66424525785499,-0.00119753195345899,
25.0714803633902));
#22246=CARTESIAN_POINT('Origin',(0.,0.,23.));
#22247=CARTESIAN_POINT('',(-1.66854406988197,-0.000512450462931708,25.7714803633902));
#22248=CARTESIAN_POINT('',(-1.66667079046023,0.00145441940323589,25.5785196366098));
#22249=CARTESIAN_POINT('',(-1.666,2.04026156737949E-16,23.));
#22250=CARTESIAN_POINT('Ctrl Pts',(-1.66667079046023,0.00145441940323589,
25.5785196366098));
#22251=CARTESIAN_POINT('Ctrl Pts',(-1.66764896339718,0.108321756637489,
25.5713637655485));
#22252=CARTESIAN_POINT('Ctrl Pts',(-1.65825057352537,0.215017733667649,
25.5642078944873));
#22253=CARTESIAN_POINT('Ctrl Pts',(-1.63785151142752,0.31956732843442,25.557052023426));
#22254=CARTESIAN_POINT('Ctrl Pts',(-1.53225004769563,0.86079761573817,25.5200076507622));
#22255=CARTESIAN_POINT('Ctrl Pts',(-1.13184096675627,1.34450688726362,25.4829632780983));
#22256=CARTESIAN_POINT('Ctrl Pts',(-0.619859344020208,1.54934026105344,
25.4459189054345));
#22257=CARTESIAN_POINT('Ctrl Pts',(-0.107877721284147,1.75417363484326,
25.4088745327706));
#22258=CARTESIAN_POINT('Ctrl Pts',(0.515676443248609,1.68013111089743,25.3718301601067));
#22259=CARTESIAN_POINT('Ctrl Pts',(0.965452492460973,1.36109600531707,25.3347857874429));
#22260=CARTESIAN_POINT('Ctrl Pts',(1.41522854167333,1.04206089973671,25.297741414779));
#22261=CARTESIAN_POINT('Ctrl Pts',(1.69122647556531,0.478033212521821,25.2606970421152));
#22262=CARTESIAN_POINT('Ctrl Pts',(1.66714420800178,-0.0728768867017734,
25.2236526694514));
#22263=CARTESIAN_POINT('Ctrl Pts',(1.64306194043825,-0.623786985925368,
25.1866082967875));
#22264=CARTESIAN_POINT('Ctrl Pts',(1.31889947141923,-1.16157949715767,25.1495639241236));
#22265=CARTESIAN_POINT('Ctrl Pts',(0.842999926222902,-1.44014998360507,
25.1125195514598));
#22266=CARTESIAN_POINT('Ctrl Pts',(0.367100381026566,-1.71872047005247,
25.0754751787959));
#22267=CARTESIAN_POINT('Ctrl Pts',(-0.260536240347081,-1.73806893171496,
25.0384308061321));
#22268=CARTESIAN_POINT('Ctrl Pts',(-0.752691068189035,-1.48934113176189,
25.0013864334682));
#22269=CARTESIAN_POINT('Ctrl Pts',(-1.24484589603098,-1.24061333180882,
24.9643420608044));
#22270=CARTESIAN_POINT('Ctrl Pts',(-1.60151893034123,-0.723809270240203,
24.9272976881405));
#22271=CARTESIAN_POINT('Ctrl Pts',(-1.65948957136256,-0.175428656234587,
24.8902533154767));
#22272=CARTESIAN_POINT('Ctrl Pts',(-1.66561023906039,-0.117529425673589,
24.8863420891877));
#22273=CARTESIAN_POINT('Ctrl Pts',(-1.66840109179986,-0.059278192319831,
24.8824308628988));
#22274=CARTESIAN_POINT('Ctrl Pts',(-1.66799179081971,-0.000987328612398951,
24.8785196366098));
#22275=CARTESIAN_POINT('Ctrl Pts',(-1.66424525785499,-0.00119753195345899,
25.0714803633902));
#22276=CARTESIAN_POINT('Ctrl Pts',(-1.66553641439486,-0.195365996377658,
25.0844338656919));
#22277=CARTESIAN_POINT('Ctrl Pts',(-1.6341480123673,-0.389130213177341,
25.0973873679937));
#22278=CARTESIAN_POINT('Ctrl Pts',(-1.56824460840503,-0.570341953455574,
25.1103408702954));
#22279=CARTESIAN_POINT('Ctrl Pts',(-1.37977432451382,-1.08857054380597,
25.1473852429593));
#22280=CARTESIAN_POINT('Ctrl Pts',(-0.909025425633515,-1.50413955169827,
25.1844296156231));
#22281=CARTESIAN_POINT('Ctrl Pts',(-0.371421872139759,-1.62687642080162,
25.221473988287));
#22282=CARTESIAN_POINT('Ctrl Pts',(0.166181681353993,-1.74961328990496,
25.2585183609509));
#22283=CARTESIAN_POINT('Ctrl Pts',(0.770639889461195,-1.57951802021935,
25.2955627336147));
#22284=CARTESIAN_POINT('Ctrl Pts',(1.16534078053029,-1.19442955459708,25.3326071062786));
#22285=CARTESIAN_POINT('Ctrl Pts',(1.56004167159939,-0.809341088974802,
25.3696514789424));
#22286=CARTESIAN_POINT('Ctrl Pts',(1.74498524563038,-0.209259427415868,
25.4066958516063));
#22287=CARTESIAN_POINT('Ctrl Pts',(1.63553768349278,0.331206252261941,25.4437402242701));
#22288=CARTESIAN_POINT('Ctrl Pts',(1.52609012135517,0.871671931939749,25.480784596934));
#22289=CARTESIAN_POINT('Ctrl Pts',(1.12225142304897,1.35252162973643,25.5178289695978));
#22290=CARTESIAN_POINT('Ctrl Pts',(0.608826124386921,1.55370906090346,25.5548733422617));
#22291=CARTESIAN_POINT('Ctrl Pts',(0.0954008257248699,1.75489649207049,
25.5919177149255));
#22292=CARTESIAN_POINT('Ctrl Pts',(-0.527611073293032,1.67642165660788,
25.6289620875894));
#22293=CARTESIAN_POINT('Ctrl Pts',(-0.975107066920903,1.35419618360633,
25.6660064602532));
#22294=CARTESIAN_POINT('Ctrl Pts',(-1.3998152901679,1.04837934932822,25.7011644279656));
#22295=CARTESIAN_POINT('Ctrl Pts',(-1.66642801081486,0.523004752093186,
25.7363223956779));
#22296=CARTESIAN_POINT('Ctrl Pts',(-1.66854406988197,-0.000512450462931708,
25.7714803633902));
#22297=CARTESIAN_POINT('Origin',(0.,0.,23.));
#22298=CARTESIAN_POINT('',(-1.66575472391166,0.00152194406742107,26.4714803633902));
#22299=CARTESIAN_POINT('',(-1.6632751401947,7.36886941808092E-5,26.2785196366098));
#22300=CARTESIAN_POINT('',(-1.666,2.04026156737949E-16,23.));
#22301=CARTESIAN_POINT('Ctrl Pts',(-1.6632751401947,7.36886941808092E-5,
26.2785196366098));
#22302=CARTESIAN_POINT('Ctrl Pts',(-1.66338307846009,0.273628708276909,
26.2602966681983));
#22303=CARTESIAN_POINT('Ctrl Pts',(-1.59965833684018,0.54713637489195,26.2420736997869));
#22304=CARTESIAN_POINT('Ctrl Pts',(-1.47182530479114,0.786391202256148,
26.2238507313754));
#22305=CARTESIAN_POINT('Ctrl Pts',(-1.21196124910893,1.27275790093975,26.1868063587115));
#22306=CARTESIAN_POINT('Ctrl Pts',(-0.687173720229887,1.61757689837527,
26.1497619860477));
#22307=CARTESIAN_POINT('Ctrl Pts',(-0.137615819036478,1.66305223528393,
26.1127176133838));
#22308=CARTESIAN_POINT('Ctrl Pts',(0.411942082156932,1.70852757219258,26.07567324072));
#22309=CARTESIAN_POINT('Ctrl Pts',(0.986270355664704,1.45465924857437,26.0386288680561));
#22310=CARTESIAN_POINT('Ctrl Pts',(1.32254508083313,1.01762240543881,26.0015844953923));
#22311=CARTESIAN_POINT('Ctrl Pts',(1.65881980600156,0.580585562303244,25.9645401227284));
#22312=CARTESIAN_POINT('Ctrl Pts',(1.75704098283065,-0.0396198003496655,
25.9274957500645));
#22313=CARTESIAN_POINT('Ctrl Pts',(1.57226066784314,-0.559175503069151,
25.8904513774007));
#22314=CARTESIAN_POINT('Ctrl Pts',(1.38748035285563,-1.07873120578864,25.8534070047368));
#22315=CARTESIAN_POINT('Ctrl Pts',(0.919698546051532,-1.4976372485747,25.816362632073));
#22316=CARTESIAN_POINT('Ctrl Pts',(0.382981408073537,-1.62419398224651,
25.7793182594092));
#22317=CARTESIAN_POINT('Ctrl Pts',(-0.153735729904462,-1.75075071591832,
25.7422738867453));
#22318=CARTESIAN_POINT('Ctrl Pts',(-0.759388199056355,-1.58495814047587,
25.7052295140814));
#22319=CARTESIAN_POINT('Ctrl Pts',(-1.15681751037009,-1.20268620121362,
25.6681851414176));
#22320=CARTESIAN_POINT('Ctrl Pts',(-1.47747529869075,-0.894257831459795,
25.638296639815));
#22321=CARTESIAN_POINT('Ctrl Pts',(-1.6625851769628,-0.444906974317528,
25.6084081382124));
#22322=CARTESIAN_POINT('Ctrl Pts',(-1.66667079046023,0.00145441940323589,
25.5785196366098));
#22323=CARTESIAN_POINT('Ctrl Pts',(-1.66854406988197,-0.000512450462931708,
25.7714803633902));
#22324=CARTESIAN_POINT('Ctrl Pts',(-1.66865760728364,-0.0286018284153655,
25.7733667683417));
#22325=CARTESIAN_POINT('Ctrl Pts',(-1.66800969269827,-0.0566858591665887,
25.7752531732933));
#22326=CARTESIAN_POINT('Ctrl Pts',(-1.66658389074195,-0.084730341556093,
25.7771395782448));
#22327=CARTESIAN_POINT('Ctrl Pts',(-1.63858463269728,-0.635455283176455,
25.8141839509086));
#22328=CARTESIAN_POINT('Ctrl Pts',(-1.31060602837012,-1.1709290558767,25.8512283235725));
#22329=CARTESIAN_POINT('Ctrl Pts',(-0.832737541654405,-1.44610832319883,
25.8882726962363));
#22330=CARTESIAN_POINT('Ctrl Pts',(-0.354869054938685,-1.72128759052096,
25.9253170689002));
#22331=CARTESIAN_POINT('Ctrl Pts',(0.272889314165587,-1.73617235246498,
25.9623614415641));
#22332=CARTESIAN_POINT('Ctrl Pts',(0.763262981787752,-1.48395104913065,
25.9994058142279));
#22333=CARTESIAN_POINT('Ctrl Pts',(1.25363664940992,-1.23172974579632,26.0364501868918));
#22334=CARTESIAN_POINT('Ctrl Pts',(1.60662561554998,-0.712402377183643,
26.0734945595556));
#22335=CARTESIAN_POINT('Ctrl Pts',(1.66069518255521,-0.163623367250885,
26.1105389322195));
#22336=CARTESIAN_POINT('Ctrl Pts',(1.71476474956044,0.38515564268187,26.1475833048833));
#22337=CARTESIAN_POINT('Ctrl Pts',(1.46991491743084,0.963386293934705,26.1846276775472));
#22338=CARTESIAN_POINT('Ctrl Pts',(1.03819378793103,1.30645886067622,26.221672050211));
#22339=CARTESIAN_POINT('Ctrl Pts',(0.606472658431218,1.64953142741774,26.2587164228749));
#22340=CARTESIAN_POINT('Ctrl Pts',(-0.01211976843881,1.75744590964794,26.2957607955387));
#22341=CARTESIAN_POINT('Ctrl Pts',(-0.534503424332941,1.58081851723447,
26.3328051682026));
#22342=CARTESIAN_POINT('Ctrl Pts',(-1.05688708022707,1.404191124821,26.3698495408664));
#22343=CARTESIAN_POINT('Ctrl Pts',(-1.4830619651453,0.943021857763867,26.4068939135303));
#22344=CARTESIAN_POINT('Ctrl Pts',(-1.61800206476684,0.408350847098134,
26.4439382861942));
#22345=CARTESIAN_POINT('Ctrl Pts',(-1.65144421691543,0.275843539498134,
26.4531189785928));
#22346=CARTESIAN_POINT('Ctrl Pts',(-1.66699886974927,0.138821790441243,
26.4622996709915));
#22347=CARTESIAN_POINT('Ctrl Pts',(-1.66575472391166,0.00152194406742107,
26.4714803633902));
#22348=CARTESIAN_POINT('Origin',(0.,0.,23.));
#22349=CARTESIAN_POINT('',(-1.66337010699017,-0.000419830789558373,27.1714803633902));
#22350=CARTESIAN_POINT('',(-1.66640033905111,-0.0014929403423002,26.9785196366098));
#22351=CARTESIAN_POINT('',(-1.666,2.04026156737949E-16,23.));
#22352=CARTESIAN_POINT('Ctrl Pts',(-1.66640033905111,-0.0014929403423002,
26.9785196366098));
#22353=CARTESIAN_POINT('Ctrl Pts',(-1.66236155042919,0.436113957710351,
26.9492295708481));
#22354=CARTESIAN_POINT('Ctrl Pts',(-1.48537353306325,0.87661185904339,26.9199395050864));
#22355=CARTESIAN_POINT('Ctrl Pts',(-1.17604733024994,1.18388915163694,26.8906494393248));
#22356=CARTESIAN_POINT('Ctrl Pts',(-0.784829528796659,1.57251561053903,
26.8536050666609));
#22357=CARTESIAN_POINT('Ctrl Pts',(-0.181927270299917,1.74804611280028,
26.816560693997));
#22358=CARTESIAN_POINT('Ctrl Pts',(0.356759509300449,1.63015444211313,26.7795163213332));
#22359=CARTESIAN_POINT('Ctrl Pts',(0.895446288900814,1.51226277142598,26.7424719486693));
#22360=CARTESIAN_POINT('Ctrl Pts',(1.36991758960481,1.10094892779044,26.7054275760055));
#22361=CARTESIAN_POINT('Ctrl Pts',(1.56304600538008,0.584438222746841,26.6683832033416));
#22362=CARTESIAN_POINT('Ctrl Pts',(1.75617442115535,0.0679275177032342,
26.6313388306778));
#22363=CARTESIAN_POINT('Ctrl Pts',(1.6679599520019,-0.553780048748435,26.5942944580139));
#22364=CARTESIAN_POINT('Ctrl Pts',(1.33877127573794,-0.996178860214455,
26.55725008535));
#22365=CARTESIAN_POINT('Ctrl Pts',(1.00958259947398,-1.43857767168047,26.5202057126862));
#22366=CARTESIAN_POINT('Ctrl Pts',(0.439419716099504,-1.70166772816084,
26.4831613400223));
#22367=CARTESIAN_POINT('Ctrl Pts',(-0.110799618615914,-1.66505384167596,
26.4461169673585));
#22368=CARTESIAN_POINT('Ctrl Pts',(-0.661018953331337,-1.62843995519108,
26.4090725946946));
#22369=CARTESIAN_POINT('Ctrl Pts',(-1.1912947393877,-1.29212212574094,26.3720282220308));
#22370=CARTESIAN_POINT('Ctrl Pts',(-1.4589623411732,-0.810006011050031,
26.3349838493669));
#22371=CARTESIAN_POINT('Ctrl Pts',(-1.59495816931649,-0.565053764901262,
26.3161624451146));
#22372=CARTESIAN_POINT('Ctrl Pts',(-1.66316365727483,-0.282464781031254,
26.2973410408622));
#22373=CARTESIAN_POINT('Ctrl Pts',(-1.6632751401947,7.36886941808092E-5,
26.2785196366098));
#22374=CARTESIAN_POINT('Ctrl Pts',(-1.66575472391166,0.00152194406742107,
26.4714803633902));
#22375=CARTESIAN_POINT('Ctrl Pts',(-1.66197870350743,-0.415187259735411,
26.4993440436554));
#22376=CARTESIAN_POINT('Ctrl Pts',(-1.50346207181111,-0.834458131765972,
26.5272077239205));
#22377=CARTESIAN_POINT('Ctrl Pts',(-1.22064153164464,-1.13785559215971,
26.5550714041857));
#22378=CARTESIAN_POINT('Ctrl Pts',(-0.844635584576064,-1.54121826647749,
26.5921157768495));
#22379=CARTESIAN_POINT('Ctrl Pts',(-0.24891837611407,-1.73977086083872,
26.6291601495134));
#22380=CARTESIAN_POINT('Ctrl Pts',(0.29389817533508,-1.64265180536657,26.6662045221773));
#22381=CARTESIAN_POINT('Ctrl Pts',(0.836714726784226,-1.54553274989443,
26.7032488948411));
#22382=CARTESIAN_POINT('Ctrl Pts',(1.32663062122053,-1.15274204458891,26.740293267505));
#22383=CARTESIAN_POINT('Ctrl Pts',(1.53945070430983,-0.64402843705345,26.7773376401688));
#22384=CARTESIAN_POINT('Ctrl Pts',(1.75227078739912,-0.135314829517993,
26.8143820128327));
#22385=CARTESIAN_POINT('Ctrl Pts',(1.68799505914141,0.489321680247402,26.8514263854965));
#22386=CARTESIAN_POINT('Ctrl Pts',(1.37603735693171,0.944035114977717,26.8884707581604));
#22387=CARTESIAN_POINT('Ctrl Pts',(1.06407965472201,1.39874854970803,26.9255151308242));
#22388=CARTESIAN_POINT('Ctrl Pts',(0.504439978560328,1.68353890940327,26.9625595034881));
#22389=CARTESIAN_POINT('Ctrl Pts',(-0.0467795406218917,1.66808055482026,
26.9996038761519));
#22390=CARTESIAN_POINT('Ctrl Pts',(-0.597999059804111,1.65262220023726,
27.0366482488158));
#22391=CARTESIAN_POINT('Ctrl Pts',(-1.14079842200687,1.33691513137601,27.0736926214796));
#22392=CARTESIAN_POINT('Ctrl Pts',(-1.42678195981814,0.865433050682779,
27.1107369941435));
#22393=CARTESIAN_POINT('Ctrl Pts',(-1.58309543279269,0.607729400876687,
27.1309847838924));
#22394=CARTESIAN_POINT('Ctrl Pts',(-1.66268467615298,0.303487661744212,
27.1512325736413));
#22395=CARTESIAN_POINT('Ctrl Pts',(-1.66337010699017,-0.000419830789558373,
27.1714803633902));
#22396=CARTESIAN_POINT('Origin',(0.,0.,23.));
#22397=CARTESIAN_POINT('',(-1.66729377121886,-0.00130306451899955,27.8714803633902));
#22398=CARTESIAN_POINT('',(-1.66818493320164,0.000858898907110364,27.6785196366098));
#22399=CARTESIAN_POINT('',(-1.666,2.04026156737949E-16,23.));
#22400=CARTESIAN_POINT('Ctrl Pts',(-1.66818493320164,0.000858898907110364,
27.6785196366098));
#22401=CARTESIAN_POINT('Ctrl Pts',(-1.66849498077994,0.0502159495743163,
27.6752068461618));
#22402=CARTESIAN_POINT('Ctrl Pts',(-1.66649429024572,0.0995475114464373,
27.6718940557137));
#22403=CARTESIAN_POINT('Ctrl Pts',(-1.66210102607721,0.148665069498833,
27.6685812652656));
#22404=CARTESIAN_POINT('Ctrl Pts',(-1.61297455169828,0.697908721749858,
27.6315368926018));
#22405=CARTESIAN_POINT('Ctrl Pts',(-1.26467543919903,1.22039286850551,27.5944925199379));
#22406=CARTESIAN_POINT('Ctrl Pts',(-0.776592464269594,1.47701887638357,
27.5574481472741));
#22407=CARTESIAN_POINT('Ctrl Pts',(-0.288509489340157,1.73364488426163,
27.5204037746102));
#22408=CARTESIAN_POINT('Ctrl Pts',(0.339357348019464,1.72441275326209,27.4833594019464));
#22409=CARTESIAN_POINT('Ctrl Pts',(0.819683955401358,1.45354708297435,27.4463150292825));
#22410=CARTESIAN_POINT('Ctrl Pts',(1.30001056278325,1.18268141268661,27.4092706566187));
#22411=CARTESIAN_POINT('Ctrl Pts',(1.63279694018742,0.650182203110672,27.3722262839548));
#22412=CARTESIAN_POINT('Ctrl Pts',(1.66575342521178,0.0997316787937973,
27.335181911291));
#22413=CARTESIAN_POINT('Ctrl Pts',(1.69870991023614,-0.450718845523074,
27.2981375386271));
#22414=CARTESIAN_POINT('Ctrl Pts',(1.4318365028807,-1.01912068458088,27.2610931659632));
#22415=CARTESIAN_POINT('Ctrl Pts',(0.987259761184316,-1.34536202632351,
27.2240487932994));
#22416=CARTESIAN_POINT('Ctrl Pts',(0.542683019487933,-1.67160336806614,
27.1870044206355));
#22417=CARTESIAN_POINT('Ctrl Pts',(-0.0795970565493923,-1.75568421249359,
27.1499600479717));
#22418=CARTESIAN_POINT('Ctrl Pts',(-0.594812875890746,-1.55912748161231,
27.1129156753079));
#22419=CARTESIAN_POINT('Ctrl Pts',(-1.1100286952321,-1.36257075073103,27.075871302644));
#22420=CARTESIAN_POINT('Ctrl Pts',(-1.51818025787748,-0.885376444541015,
27.0388269299801));
#22421=CARTESIAN_POINT('Ctrl Pts',(-1.63248936699526,-0.345918083674546,
27.0017825573163));
#22422=CARTESIAN_POINT('Ctrl Pts',(-1.65641710149505,-0.232996055569109,
26.9940282504141));
#22423=CARTESIAN_POINT('Ctrl Pts',(-1.66746957551995,-0.117345810650349,
26.986273943512));
#22424=CARTESIAN_POINT('Ctrl Pts',(-1.66640033905111,-0.0014929403423002,
26.9785196366098));
#22425=CARTESIAN_POINT('Ctrl Pts',(-1.66337010699017,-0.000419830789558373,
27.1714803633902));
#22426=CARTESIAN_POINT('Ctrl Pts',(-1.66393870712045,-0.252526725424533,
27.1882769463052));
#22427=CARTESIAN_POINT('Ctrl Pts',(-1.61020920893848,-0.504403606399881,
27.2050735292201));
#22428=CARTESIAN_POINT('Ctrl Pts',(-1.5009373747887,-0.729292911466197,
27.2218701121351));
#22429=CARTESIAN_POINT('Ctrl Pts',(-1.2599415385282,-1.22527970039674,27.2589144847989));
#22430=CARTESIAN_POINT('Ctrl Pts',(-0.748782152587401,-1.58999618573263,
27.2959588574628));
#22431=CARTESIAN_POINT('Ctrl Pts',(-0.201375822283328,-1.65654116769859,
27.3330032301266));
#22432=CARTESIAN_POINT('Ctrl Pts',(0.346030508020746,-1.72308614966455,
27.3700476027905));
#22433=CARTESIAN_POINT('Ctrl Pts',(0.929683782688092,-1.49145962826058,
27.4070919754543));
#22434=CARTESIAN_POINT('Ctrl Pts',(1.28249279779562,-1.06765799378737,27.4441363481182));
#22435=CARTESIAN_POINT('Ctrl Pts',(1.63530181290315,-0.643856359314169,
27.481180720782));
#22436=CARTESIAN_POINT('Ctrl Pts',(1.75726656845087,-0.0278796117717245,
27.5182250934459));
#22437=CARTESIAN_POINT('Ctrl Pts',(1.59257355216309,0.498388274239166,27.5552694661097));
#22438=CARTESIAN_POINT('Ctrl Pts',(1.42788053587531,1.02465616025006,27.5923138387736));
#22439=CARTESIAN_POINT('Ctrl Pts',(0.97652974775204,1.46121518472939,27.6293582114374));
#22440=CARTESIAN_POINT('Ctrl Pts',(0.445068267638841,1.60828906290049,27.6664025841013));
#22441=CARTESIAN_POINT('Ctrl Pts',(-0.0863932124743599,1.75536294107158,
27.7034469567652));
#22442=CARTESIAN_POINT('Ctrl Pts',(-0.69796538457749,1.61295167293442,27.740491329429));
#22443=CARTESIAN_POINT('Ctrl Pts',(-1.10978093456905,1.24622215767095,27.7775357020928));
#22444=CARTESIAN_POINT('Ctrl Pts',(-1.45790283612392,0.93621303778115,27.808850589192));
#22445=CARTESIAN_POINT('Ctrl Pts',(-1.66328056200809,0.465908239402866,
27.8401654762911));
#22446=CARTESIAN_POINT('Ctrl Pts',(-1.66729377121886,-0.00130306451899955,
27.8714803633902));
#22447=CARTESIAN_POINT('Origin',(0.,0.,23.));
#22448=CARTESIAN_POINT('',(-1.66745735078673,0.00120170187390745,28.5714803633902));
#22449=CARTESIAN_POINT('',(-1.6638200260918,0.000942871389988137,28.3785196366098));
#22450=CARTESIAN_POINT('',(-1.666,2.04026156737949E-16,23.));
#22451=CARTESIAN_POINT('',(1.26907087985238,1.07935865304851,29.));
#22452=CARTESIAN_POINT('Ctrl Pts',(-1.66745735078673,0.00120170187390745,
28.5714803633902));
#22453=CARTESIAN_POINT('Ctrl Pts',(-1.66350963374581,-0.471613114236158,
28.6031871242686));
#22454=CARTESIAN_POINT('Ctrl Pts',(-1.45232521651817,-0.94739347524418,
28.6348938851469));
#22455=CARTESIAN_POINT('Ctrl Pts',(-1.09656156402175,-1.25768579906275,
28.6666006460253));
#22456=CARTESIAN_POINT('Ctrl Pts',(-0.680907584926055,-1.62021366882408,
28.7036450186892));
#22457=CARTESIAN_POINT('Ctrl Pts',(-0.0678992765999901,-1.75684616353755,
28.740689391353));
#22458=CARTESIAN_POINT('Ctrl Pts',(0.462005451356146,-1.60382582725002,
28.7777337640169));
#22459=CARTESIAN_POINT('Ctrl Pts',(0.991910179312282,-1.45080549096249,
28.8147781366808));
#22460=CARTESIAN_POINT('Ctrl Pts',(1.43871132689849,-1.00813232367397,28.8518225093446));
#22461=CARTESIAN_POINT('Ctrl Pts',(1.59772575664243,-0.481085822244155,
28.8888668820085));
#22462=CARTESIAN_POINT('Ctrl Pts',(1.75674018638636,0.0459606791856584,
28.9259112546723));
#22463=CARTESIAN_POINT('Ctrl Pts',(1.62796789828802,0.657380514756762,28.9629556273361));
#22464=CARTESIAN_POINT('Ctrl Pts',(1.26907087985237,1.07935865304853,29.));
#22465=CARTESIAN_POINT('',(-1.27144765946785,1.08124504477636,29.));
#22466=CARTESIAN_POINT('Origin',(0.,0.,29.));
#22467=CARTESIAN_POINT('Ctrl Pts',(-1.27144834193525,1.08124558643403,29.));
#22468=CARTESIAN_POINT('Ctrl Pts',(-0.920624410300644,1.49274880387387,
28.9636818543909));
#22469=CARTESIAN_POINT('Ctrl Pts',(-0.350778053489151,1.71868133567313,
28.9273637087819));
#22470=CARTESIAN_POINT('Ctrl Pts',(0.186547721698795,1.65813753251397,28.8910455631728));
#22471=CARTESIAN_POINT('Ctrl Pts',(0.734618002384743,1.59638307977135,28.8540011905089));
#22472=CARTESIAN_POINT('Ctrl Pts',(1.24885411811842,1.23658083427687,28.8169568178451));
#22473=CARTESIAN_POINT('Ctrl Pts',(1.49426097077748,0.742855457794705,28.7799124451812));
#22474=CARTESIAN_POINT('Ctrl Pts',(1.73966782343655,0.249130081312535,28.7428680725174));
#22475=CARTESIAN_POINT('Ctrl Pts',(1.71624541302099,-0.378518426157325,
28.7058236998535));
#22476=CARTESIAN_POINT('Ctrl Pts',(1.43454159545344,-0.852593208110846,
28.6687793271897));
#22477=CARTESIAN_POINT('Ctrl Pts',(1.1528377778859,-1.32666799006437,28.6317349545258));
#22478=CARTESIAN_POINT('Ctrl Pts',(0.612852553166363,-1.64716904650155,
28.594690581862));
#22479=CARTESIAN_POINT('Ctrl Pts',(0.0617825081308379,-1.66757033753488,
28.5576462091981));
#22480=CARTESIAN_POINT('Ctrl Pts',(-0.489287536904685,-1.68797162856822,
28.5206018365343));
#22481=CARTESIAN_POINT('Ctrl Pts',(-1.0514424022562,-1.4082731541977,28.4835574638704));
#22482=CARTESIAN_POINT('Ctrl Pts',(-1.36747510148739,-0.956396832767403,
28.4465130912066));
#22483=CARTESIAN_POINT('Ctrl Pts',(-1.56083020008092,-0.679929901039163,
28.423848606341));
#22484=CARTESIAN_POINT('Ctrl Pts',(-1.66205596190706,-0.339012736706109,
28.4011841214754));
#22485=CARTESIAN_POINT('Ctrl Pts',(-1.6638200260918,0.000942871389988137,
28.3785196366098));
#22486=CARTESIAN_POINT('Origin',(0.,0.,30.5459252805377));
#22487=CARTESIAN_POINT('',(-2.05539098592872,0.00181257412559116,18.3540747194623));
#22488=CARTESIAN_POINT('',(-2.05290622350845,-0.00151880093680796,18.2959252805377));
#22489=CARTESIAN_POINT('',(-2.05475,1.58232769237955E-13,30.5459252805377));
#22490=CARTESIAN_POINT('',(1.81742788875943,0.958620587959298,18.));
#22491=CARTESIAN_POINT('Ctrl Pts',(-2.05290622350845,-0.00151880093680801,
18.2959252805377));
#22492=CARTESIAN_POINT('Ctrl Pts',(-2.04995766327688,0.45238457131471,18.2713722656862));
#22493=CARTESIAN_POINT('Ctrl Pts',(-1.67844748626583,1.5958979401344,18.2097748781708));
#22494=CARTESIAN_POINT('Ctrl Pts',(0.216442804381921,2.41814053114287,18.1111331179916));
#22495=CARTESIAN_POINT('Ctrl Pts',(1.4986774253635,1.56293264739877,18.0370443726639));
#22496=CARTESIAN_POINT('Ctrl Pts',(1.81742788875943,0.958620587959298,18.));
#22497=CARTESIAN_POINT('',(2.0571089891529,-0.0753984945660209,18.));
#22498=CARTESIAN_POINT('Origin',(0.,0.,18.));
#22499=CARTESIAN_POINT('Ctrl Pts',(-2.05539098592872,0.001812574125591,
18.3540747194623));
#22500=CARTESIAN_POINT('Ctrl Pts',(-2.05668615726959,0.142173868935286,
18.3464567039116));
#22501=CARTESIAN_POINT('Ctrl Pts',(-1.97955796804357,0.963669298063719,
18.3017943156971));
#22502=CARTESIAN_POINT('Ctrl Pts',(-0.873549834886296,2.26598780907704,
18.2200875548188));
#22503=CARTESIAN_POINT('Ctrl Pts',(1.41373496756836,1.96497190368407,18.109680663882));
#22504=CARTESIAN_POINT('Ctrl Pts',(2.08071254605835,0.591116081556763,18.0363181456091));
#22505=CARTESIAN_POINT('Ctrl Pts',(2.0571100610898,-0.0753985702550394,
18.));
#22506=CARTESIAN_POINT('Origin',(0.,0.,30.5459252805377));
#22507=CARTESIAN_POINT('',(-2.05138759503762,-4.97339178941181E-5,19.0540747194623));
#22508=CARTESIAN_POINT('',(-2.05798293875546,-0.000483242835675936,18.9959252805377));
#22509=CARTESIAN_POINT('',(-2.05475,1.58232769237955E-13,30.5459252805377));
#22510=CARTESIAN_POINT('Ctrl Pts',(-2.05798293875546,-0.000483242835675884,
18.9959252805377));
#22511=CARTESIAN_POINT('Ctrl Pts',(-2.05591526442115,0.653598076368698,
18.9603051683359));
#22512=CARTESIAN_POINT('Ctrl Pts',(-1.36492080142796,1.99168784117887,18.8876406834704));
#22513=CARTESIAN_POINT('Ctrl Pts',(0.91417845046059,2.24995443991895,18.7779318259409));
#22514=CARTESIAN_POINT('Ctrl Pts',(2.38596583103409,0.452399485900713,18.6667987079494));
#22515=CARTESIAN_POINT('Ctrl Pts',(1.67442227650725,-1.75934857315356,18.5556655899578));
#22516=CARTESIAN_POINT('Ctrl Pts',(-0.570385735669315,-2.36060373212415,
18.4445324719663));
#22517=CARTESIAN_POINT('Ctrl Pts',(-1.91138556361506,-1.14623593643521,
18.3579523688262));
#22518=CARTESIAN_POINT('Ctrl Pts',(-2.05440630490808,-0.232442354288971,
18.30841663835));
#22519=CARTESIAN_POINT('Ctrl Pts',(-2.05290622350845,-0.00151880093680801,
18.2959252805377));
#22520=CARTESIAN_POINT('Ctrl Pts',(-2.05138759503762,-4.97339178940834E-5,
19.0540747194623));
#22521=CARTESIAN_POINT('Ctrl Pts',(-2.05131375814071,0.34589479280389,19.0353896065614));
#22522=CARTESIAN_POINT('Ctrl Pts',(-1.80422891290684,1.37779527947084,18.9796601209967));
#22523=CARTESIAN_POINT('Ctrl Pts',(-0.170134977547301,2.42261514214274,
18.8868862627681));
#22524=CARTESIAN_POINT('Ctrl Pts',(1.9430184348445,1.45691614743391,18.7757531447766));
#22525=CARTESIAN_POINT('Ctrl Pts',(2.27790227156009,-0.842194003777161,
18.664620026785));
#22526=CARTESIAN_POINT('Ctrl Pts',(0.52784999826971,-2.37052551568832,18.5534869087934));
#22527=CARTESIAN_POINT('Ctrl Pts',(-1.55203386772556,-1.77316213953964,
18.4499718063526));
#22528=CARTESIAN_POINT('Ctrl Pts',(-2.05038808535102,-0.540365576925945,
18.3835010765755));
#22529=CARTESIAN_POINT('Ctrl Pts',(-2.05539098592872,0.001812574125591,
18.3540747194623));
#22530=CARTESIAN_POINT('Origin',(0.,0.,30.5459252805377));
#22531=CARTESIAN_POINT('',(-2.05550167136418,-0.00180630479153662,19.7540747194623));
#22532=CARTESIAN_POINT('',(-2.05419418048317,0.00186544829068187,19.6959252805377));
#22533=CARTESIAN_POINT('',(-2.05475,1.58232769237955E-13,30.5459252805377));
#22534=CARTESIAN_POINT('Ctrl Pts',(-2.05419418048317,0.00186544829068198,
19.6959252805377));
#22535=CARTESIAN_POINT('Ctrl Pts',(-2.05577927155616,0.179783416190269,
19.6862824436496));
#22536=CARTESIAN_POINT('Ctrl Pts',(-1.95316269205233,1.03939956340346,19.6395952340976));
#22537=CARTESIAN_POINT('Ctrl Pts',(-0.74919538183736,2.31013209082318,19.5558636518818));
#22538=CARTESIAN_POINT('Ctrl Pts',(1.53447086719707,1.88239297517548,19.4447305338903));
#22539=CARTESIAN_POINT('Ctrl Pts',(2.41372487585493,-0.268184847585669,
19.3335974158987));
#22540=CARTESIAN_POINT('Ctrl Pts',(1.08385077038562,-2.17331209936668,19.2224642979071));
#22541=CARTESIAN_POINT('Ctrl Pts',(-1.23802140067364,-2.08933327590159,
19.1113311799156));
#22542=CARTESIAN_POINT('Ctrl Pts',(-2.04576099362511,-0.732944466062138,
19.0358181741258));
#22543=CARTESIAN_POINT('Ctrl Pts',(-2.05806561414924,-0.0266365058203424,
18.9973495409998));
#22544=CARTESIAN_POINT('Ctrl Pts',(-2.05798293875546,-0.000483242835675884,
18.9959252805377));
#22545=CARTESIAN_POINT('Ctrl Pts',(-2.05550167136418,-0.00180630479153664,
19.7540747194623));
#22546=CARTESIAN_POINT('Ctrl Pts',(-2.05047133330275,0.546252139932218,
19.7243225092112));
#22547=CARTESIAN_POINT('Ctrl Pts',(-1.54308293551855,1.7849188256759,19.6575259262963));
#22548=CARTESIAN_POINT('Ctrl Pts',(0.548689842456826,2.36578558927548,19.5536849707175));
#22549=CARTESIAN_POINT('Ctrl Pts',(2.28517284872419,0.82218308608128,19.4425518527259));
#22550=CARTESIAN_POINT('Ctrl Pts',(1.93017685695003,-1.47391342438527,19.3314187347344));
#22551=CARTESIAN_POINT('Ctrl Pts',(-0.191395150412758,-2.42102695967158,
19.2202856167428));
#22552=CARTESIAN_POINT('Ctrl Pts',(-1.81053783300646,-1.36563128814009,
19.1278376116521));
#22553=CARTESIAN_POINT('Ctrl Pts',(-2.05146014427923,-0.339961270088832,
19.0724339792253));
#22554=CARTESIAN_POINT('Ctrl Pts',(-2.05138759503762,-4.97339178940834E-5,
19.0540747194623));
#22555=CARTESIAN_POINT('Origin',(0.,0.,30.5459252805377));
#22556=CARTESIAN_POINT('',(-2.05726314523298,0.00118285322517675,20.4540747194623));
#22557=CARTESIAN_POINT('',(-2.05157916456917,-0.000651383278007832,20.3959252805377));
#22558=CARTESIAN_POINT('',(-2.05475,1.58232769237955E-13,30.5459252805377));
#22559=CARTESIAN_POINT('Ctrl Pts',(-2.05157916456917,-0.000651383278007581,
20.3959252805377));
#22560=CARTESIAN_POINT('Ctrl Pts',(-2.05048915160027,0.382692054795739,
20.3752153462994));
#22561=CARTESIAN_POINT('Ctrl Pts',(-1.76331355358747,1.45324785939933,20.3174610393972));
#22562=CARTESIAN_POINT('Ctrl Pts',(-0.037864870345937,2.42828507097424,
20.2226623598312));
#22563=CARTESIAN_POINT('Ctrl Pts',(2.01954547577021,1.34886554398611,20.1115292418396));
#22564=CARTESIAN_POINT('Ctrl Pts',(2.22858823263633,-0.965088791301547,
20.0003961238481));
#22565=CARTESIAN_POINT('Ctrl Pts',(0.397939478909703,-2.39575593384446,
19.8892630058565));
#22566=CARTESIAN_POINT('Ctrl Pts',(-1.60647516920198,-1.69985232818512,
19.787772724753));
#22567=CARTESIAN_POINT('Ctrl Pts',(-2.04968991164107,-0.503714560904521,
19.7233268163134));
#22568=CARTESIAN_POINT('Ctrl Pts',(-2.05419418048317,0.00186544829068198,
19.6959252805377));
#22569=CARTESIAN_POINT('Ctrl Pts',(-2.05726314523298,0.00118285322517685,
20.4540747194623));
#22570=CARTESIAN_POINT('Ctrl Pts',(-2.05773933212956,0.0705652968257603,
20.4502997845249));
#22571=CARTESIAN_POINT('Ctrl Pts',(-2.02307416841907,0.820333420006341,
20.4094804769236));
#22572=CARTESIAN_POINT('Ctrl Pts',(-1.10336950687639,2.16346419607446,20.3316167966584));
#22573=CARTESIAN_POINT('Ctrl Pts',(1.21915193180051,2.10039762278245,20.2204836786668));
#22574=CARTESIAN_POINT('Ctrl Pts',(2.42585752542742,0.114964471039976,20.1093505606753));
#22575=CARTESIAN_POINT('Ctrl Pts',(1.41232285348001,-1.97568868333651,19.9982174426837));
#22576=CARTESIAN_POINT('Ctrl Pts',(-0.893825325748239,-2.2581138043306,
19.8870843246922));
#22577=CARTESIAN_POINT('Ctrl Pts',(-1.98352412167925,-0.95150867536627,
19.8057034169517));
#22578=CARTESIAN_POINT('Ctrl Pts',(-2.05673458958522,-0.136133507943197,
19.7613668818751));
#22579=CARTESIAN_POINT('Ctrl Pts',(-2.05550167136418,-0.00180630479153664,
19.7540747194623));
#22580=CARTESIAN_POINT('Origin',(0.,0.,30.5459252805377));
#22581=CARTESIAN_POINT('',(-2.0519251869176,0.00105510962586416,21.1540747194623));
#22582=CARTESIAN_POINT('',(-2.0565803487625,-0.00152072744175304,21.0959252805377));
#22583=CARTESIAN_POINT('',(-2.05475,1.58232769237955E-13,30.5459252805377));
#22584=CARTESIAN_POINT('Ctrl Pts',(-2.0565803487625,-0.00152072744175287,
21.0959252805377));
#22585=CARTESIAN_POINT('Ctrl Pts',(-2.0517372846152,0.583041769572967,21.0641482489491));
#22586=CARTESIAN_POINT('Ctrl Pts',(-1.48486127333146,1.8572733659222,20.9953268446968));
#22587=CARTESIAN_POINT('Ctrl Pts',(0.676803113364313,2.33236782238435,20.8894610677805));
#22588=CARTESIAN_POINT('Ctrl Pts',(2.3265840468287,0.696425723269271,20.778327949789));
#22589=CARTESIAN_POINT('Ctrl Pts',(1.84698368557056,-1.57691260826926,20.6671948317974));
#22590=CARTESIAN_POINT('Ctrl Pts',(-0.323048838197336,-2.40699845512473,
20.5560617138059));
#22591=CARTESIAN_POINT('Ctrl Pts',(-1.84812165816893,-1.28994678035528,
20.4656385300526));
#22592=CARTESIAN_POINT('Ctrl Pts',(-2.0524388848135,-0.303003853981133,
20.4122597189632));
#22593=CARTESIAN_POINT('Ctrl Pts',(-2.05157916456917,-0.000651383278007581,
20.3959252805377));
#22594=CARTESIAN_POINT('Ctrl Pts',(-2.0519251869176,0.00105510962586441,
21.1540747194623));
#22595=CARTESIAN_POINT('Ctrl Pts',(-2.05320297921829,0.275667101474611,
21.1392326871747));
#22596=CARTESIAN_POINT('Ctrl Pts',(-1.87404526463701,1.23408694721642,21.0873462822232));
#22597=CARTESIAN_POINT('Ctrl Pts',(-0.419493009128206,2.39207592060309,
20.9984155046077));
#22598=CARTESIAN_POINT('Ctrl Pts',(1.7821373527842,1.64984485657254,20.8872823866162));
#22599=CARTESIAN_POINT('Ctrl Pts',(2.35268546495377,-0.602389157518069,
20.7761492686246));
#22600=CARTESIAN_POINT('Ctrl Pts',(0.769963239246222,-2.30329290471873,
20.6650161506331));
#22601=CARTESIAN_POINT('Ctrl Pts',(-1.43976118523263,-1.90996263191677,
20.557657967579));
#22602=CARTESIAN_POINT('Ctrl Pts',(-2.05306639202681,-0.6103018279468,20.4873441571887));
#22603=CARTESIAN_POINT('Ctrl Pts',(-2.05726314523298,0.00118285322517685,
20.4540747194623));
#22604=CARTESIAN_POINT('Origin',(0.,0.,30.5459252805377));
#22605=CARTESIAN_POINT('',(-2.05341424816682,-0.00175368872599717,21.8540747194623));
#22606=CARTESIAN_POINT('',(-2.05630909038221,0.00161611837171143,21.7959252805377));
#22607=CARTESIAN_POINT('',(-2.05475,1.58232769237955E-13,30.5459252805377));
#22608=CARTESIAN_POINT('Ctrl Pts',(-2.05630909038221,0.00161611837171153,
21.7959252805377));
#22609=CARTESIAN_POINT('Ctrl Pts',(-2.05723022072092,0.108343634502101,
21.7901255242628));
#22610=CARTESIAN_POINT('Ctrl Pts',(-2.00114645477151,0.895793945750412,
21.747281395324));
#22611=CARTESIAN_POINT('Ctrl Pts',(-0.983827005302519,2.22037981812055,
21.6673928937214));
#22612=CARTESIAN_POINT('Ctrl Pts',(1.33180612413638,2.03083592660637,21.5562597757299));
#22613=CARTESIAN_POINT('Ctrl Pts',(2.42851786940399,-0.0174089378669135,
21.4451266577383));
#22614=CARTESIAN_POINT('Ctrl Pts',(1.30255447502931,-2.04972045718415,21.3339935397468));
#22615=CARTESIAN_POINT('Ctrl Pts',(-1.01555804287549,-2.20604713789681,
21.2228604217552));
#22616=CARTESIAN_POINT('Ctrl Pts',(-2.00713056245277,-0.875936710560245,
21.1435043353522));
#22617=CARTESIAN_POINT('Ctrl Pts',(-2.05738313207606,-0.0984174449039837,
21.101192621613));
#22618=CARTESIAN_POINT('Ctrl Pts',(-2.0565803487625,-0.00152072744175287,
21.0959252805377));
#22619=CARTESIAN_POINT('Ctrl Pts',(-2.05341424816682,-0.0017536887259971,
21.8540747194623));
#22620=CARTESIAN_POINT('Ctrl Pts',(-2.04952656050121,0.476751074253768,
21.8281655898244));
#22621=CARTESIAN_POINT('Ctrl Pts',(-1.64443235649635,1.64534626353278,21.7652120875227));
#22622=CARTESIAN_POINT('Ctrl Pts',(0.301364750346359,2.40980930405301,21.6652142125571));
#22623=CARTESIAN_POINT('Ctrl Pts',(2.18801481710634,1.05384664671037,21.5540810945656));
#22624=CARTESIAN_POINT('Ctrl Pts',(2.07210760382199,-1.2666379407027,21.442947976574));
#22625=CARTESIAN_POINT('Ctrl Pts',(0.0597259541680415,-2.42784563039867,
21.3318148585825));
#22626=CARTESIAN_POINT('Ctrl Pts',(-1.73126155251785,-1.50867220106731,
21.2355237728785));
#22627=CARTESIAN_POINT('Ctrl Pts',(-2.05001372499377,-0.409739638440497,
21.1762770598385));
#22628=CARTESIAN_POINT('Ctrl Pts',(-2.0519251869176,0.00105510962586441,
21.1540747194623));
#22629=CARTESIAN_POINT('Origin',(0.,0.,30.5459252805377));
#22630=CARTESIAN_POINT('',(-2.05812459253004,-2.33768028169005E-5,22.5540747194623));
#22631=CARTESIAN_POINT('',(-2.05149685129519,0.000497173714744954,22.4959252805377));
#22632=CARTESIAN_POINT('',(-2.05475,1.58232769237955E-13,30.5459252805377));
#22633=CARTESIAN_POINT('Ctrl Pts',(-2.05149685129519,0.000497173714744739,
22.4959252805377));
#22634=CARTESIAN_POINT('Ctrl Pts',(-2.05217289056284,0.312735992683416,
22.4790584269126));
#22635=CARTESIAN_POINT('Ctrl Pts',(-1.83851165054927,1.30986170311779,22.4251472006236));
#22636=CARTESIAN_POINT('Ctrl Pts',(-0.288508063209722,2.41138242727093,
22.3341916016708));
#22637=CARTESIAN_POINT('Ctrl Pts',(1.86940104446612,1.5502715400977,22.2230584836792));
#22638=CARTESIAN_POINT('Ctrl Pts',(2.31636073733878,-0.729708878666279,
22.1119253656877));
#22639=CARTESIAN_POINT('Ctrl Pts',(0.643295912328174,-2.34183101061307,
22.0007922476961));
#22640=CARTESIAN_POINT('Ctrl Pts',(-1.50049922779959,-1.83833993148199,
21.8954588859795));
#22641=CARTESIAN_POINT('Ctrl Pts',(-2.05134675011945,-0.573349473558514,
21.8271698969266));
#22642=CARTESIAN_POINT('Ctrl Pts',(-2.05630909038221,0.00161611837171153,
21.7959252805377));
#22643=CARTESIAN_POINT('Ctrl Pts',(-2.05812446424055,-2.33759141173628E-5,
22.5540747194623));
#22644=CARTESIAN_POINT('Ctrl Pts',(-2.05801030910826,0.678835990556527,
22.5170984924742));
#22645=CARTESIAN_POINT('Ctrl Pts',(-1.31953539558407,2.03801862491187,22.4430778928222));
#22646=CARTESIAN_POINT('Ctrl Pts',(0.995655084428766,2.21510102422083,22.3320129205065));
#22647=CARTESIAN_POINT('Ctrl Pts',(2.40100336441846,0.364944432351608,22.2208798025149));
#22648=CARTESIAN_POINT('Ctrl Pts',(1.60885886272077,-1.81922366807872,22.1097466845233));
#22649=CARTESIAN_POINT('Ctrl Pts',(-0.655776594206566,-2.33836666353754,
21.9986135665318));
#22650=CARTESIAN_POINT('Ctrl Pts',(-1.93217795383359,-1.0952630718048,21.9133895781781));
#22651=CARTESIAN_POINT('Ctrl Pts',(-2.05508510116615,-0.207405785084765,
21.8652099624883));
#22652=CARTESIAN_POINT('Ctrl Pts',(-2.05341424816682,-0.0017536887259971,
21.8540747194623));
#22653=CARTESIAN_POINT('Origin',(0.,0.,30.5459252805377));
#22654=CARTESIAN_POINT('',(-2.05348239882457,0.00176844693486861,23.2540747194623));
#22655=CARTESIAN_POINT('',(-2.05448631486103,-0.00187785994470203,23.1959252805377));
#22656=CARTESIAN_POINT('',(-2.05475,1.58232769237955E-13,30.5459252805377));
#22657=CARTESIAN_POINT('Ctrl Pts',(-2.05448631486103,-0.00187785994470195,
23.1959252805377));
#22658=CARTESIAN_POINT('Ctrl Pts',(-2.04980780123993,0.513338964801136,
23.1679913295623));
#22659=CARTESIAN_POINT('Ctrl Pts',(-1.59250660598457,1.71920910668239,23.1030130059232));
#22660=CARTESIAN_POINT('Ctrl Pts',(0.43224489671947,2.38980469125578,23.0009903096202));
#22661=CARTESIAN_POINT('Ctrl Pts',(2.24219509588329,0.933039798232153,22.8898571916286));
#22662=CARTESIAN_POINT('Ctrl Pts',(2.00000009135574,-1.37767984222214,22.778724073637));
#22663=CARTESIAN_POINT('Ctrl Pts',(-0.072673716017103,-2.42749266612454,
22.6675909556455));
#22664=CARTESIAN_POINT('Ctrl Pts',(-1.77435552575201,-1.43343346508708,
22.573324691279));
#22665=CARTESIAN_POINT('Ctrl Pts',(-2.05068811746153,-0.373028609718886,
22.5161027995764));
#22666=CARTESIAN_POINT('Ctrl Pts',(-2.05149685129519,0.000497173714744739,
22.4959252805377));
#22667=CARTESIAN_POINT('Ctrl Pts',(-2.05348239882457,0.00176844693486848,
23.2540747194623));
#22668=CARTESIAN_POINT('Ctrl Pts',(-2.05515072772512,0.204886378054778,
23.2430757677879));
#22669=CARTESIAN_POINT('Ctrl Pts',(-1.93415066850296,1.09015999771089,23.1950324434495));
#22670=CARTESIAN_POINT('Ctrl Pts',(-0.664354069263913,2.33594419139362,
23.1099447464474));
#22671=CARTESIAN_POINT('Ctrl Pts',(1.60217141007485,1.82511598738049,22.9988116284558));
#22672=CARTESIAN_POINT('Ctrl Pts',(2.40232655406092,-0.356130204148507,
22.8876785104642));
#22673=CARTESIAN_POINT('Ctrl Pts',(1.00377788111867,-2.21143201569255,22.7765453924727));
#22674=CARTESIAN_POINT('Ctrl Pts',(-1.3134678169358,-2.04274420535881,22.6654122744811));
#22675=CARTESIAN_POINT('Ctrl Pts',(-2.0575570926931,-0.68263587599728,22.5912553834777));
#22676=CARTESIAN_POINT('Ctrl Pts',(-2.05812467462379,-0.00127448599310305,
22.5541428651381));
#22677=CARTESIAN_POINT('Ctrl Pts',(-2.05812446424055,-2.33759141173628E-5,
22.5540747194623));
#22678=CARTESIAN_POINT('Origin',(0.,0.,30.5459252805377));
#22679=CARTESIAN_POINT('',(-2.05188677382997,-0.0010204005874441,23.9540747194623));
#22680=CARTESIAN_POINT('',(-2.05787060010134,0.000654429798481389,23.8959252805377));
#22681=CARTESIAN_POINT('',(-2.05475,1.58232769237955E-13,30.5459252805377));
#22682=CARTESIAN_POINT('Ctrl Pts',(-2.05787060010134,0.000654429798481659,
23.8959252805377));
#22683=CARTESIAN_POINT('Ctrl Pts',(-2.05802039377806,0.0365895959979924,
23.893968604876));
#22684=CARTESIAN_POINT('Ctrl Pts',(-2.04088291558022,0.752714337046035,
23.8549675565504));
#22685=CARTESIAN_POINT('Ctrl Pts',(-1.20793243662604,2.10687003434831,23.7789221355611));
#22686=CARTESIAN_POINT('Ctrl Pts',(1.11489242455252,2.15754883948512,23.6677890175695));
#22687=CARTESIAN_POINT('Ctrl Pts',(2.4173238570424,0.233554026430338,23.556655899578));
#22688=CARTESIAN_POINT('Ctrl Pts',(1.50732535062721,-1.90419862421039,23.4455227815864));
#22689=CARTESIAN_POINT('Ctrl Pts',(-0.782236644429685,-2.29915374544626,
23.3343896635949));
#22690=CARTESIAN_POINT('Ctrl Pts',(-1.96032433113491,-1.01948053926428,
23.2511904965786));
#22691=CARTESIAN_POINT('Ctrl Pts',(-2.05601217248144,-0.169911466741311,
23.2050357022262));
#22692=CARTESIAN_POINT('Ctrl Pts',(-2.05448631486103,-0.00187785994470195,
23.1959252805377));
#22693=CARTESIAN_POINT('Ctrl Pts',(-2.05188677382997,-0.00102040058744382,
23.9540747194623));
#22694=CARTESIAN_POINT('Ctrl Pts',(-2.05005157165762,0.407271771044751,
23.9320086704376));
#22695=CARTESIAN_POINT('Ctrl Pts',(-1.73425658592992,1.50361854917053,23.8728982487491));
#22696=CARTESIAN_POINT('Ctrl Pts',(0.0508152693856986,2.42804847625626,
23.7767434543967));
#22697=CARTESIAN_POINT('Ctrl Pts',(2.06744504127525,1.27423412132916,23.6656103364052));
#22698=CARTESIAN_POINT('Ctrl Pts',(2.19186773754582,-1.04580945480468,23.5544772184136));
#22699=CARTESIAN_POINT('Ctrl Pts',(0.310206809340991,-2.40868705524225,
23.443344100422));
#22700=CARTESIAN_POINT('Ctrl Pts',(-1.64103861628355,-1.65033813069636,
23.343209934105));
#22701=CARTESIAN_POINT('Ctrl Pts',(-2.04953181063674,-0.479213030490258,
23.2801201404517));
#22702=CARTESIAN_POINT('Ctrl Pts',(-2.05348239882457,0.00176844693486848,
23.2540747194623));
#22703=CARTESIAN_POINT('Origin',(0.,0.,30.5459252805377));
#22704=CARTESIAN_POINT('',(-2.05720656193685,-0.00121771516567365,24.6540747194623));
#22705=CARTESIAN_POINT('',(-2.05255723160113,0.00146350343929692,24.5959252805377));
#22706=CARTESIAN_POINT('',(-2.05475,1.58232769237955E-13,30.5459252805377));
#22707=CARTESIAN_POINT('Ctrl Pts',(-2.05255723160113,0.00146350343929682,
24.5959252805377));
#22708=CARTESIAN_POINT('Ctrl Pts',(-2.05414229361448,0.242247432832211,
24.5829015075258));
#22709=CARTESIAN_POINT('Ctrl Pts',(-1.90365362879482,1.16599091497401,24.53283336185));
#22710=CARTESIAN_POINT('Ctrl Pts',(-0.536064276162042,2.36867836670812,
24.4457208435105));
#22711=CARTESIAN_POINT('Ctrl Pts',(1.69925433258817,1.73508986115085,24.3345877255189));
#22712=CARTESIAN_POINT('Ctrl Pts',(2.37934849415491,-0.486521177803125,
24.2234546075274));
#22713=CARTESIAN_POINT('Ctrl Pts',(0.881769263626921,-2.26284888554473,
24.1123214895357));
#22714=CARTESIAN_POINT('Ctrl Pts',(-1.38226358570042,-1.97331725525488,
24.0031450472059));
#22715=CARTESIAN_POINT('Ctrl Pts',(-2.05518445479657,-0.643745788400026,
23.9310129775398));
#22716=CARTESIAN_POINT('Ctrl Pts',(-2.05787060010134,0.000654429798481659,
23.8959252805377));
#22717=CARTESIAN_POINT('Ctrl Pts',(-2.05720656193685,-0.00121771516567365,
24.6540747194623));
#22718=CARTESIAN_POINT('Ctrl Pts',(-2.0529301797436,0.60780601961932,24.6209415730874));
#22719=CARTESIAN_POINT('Ctrl Pts',(-1.44395772496755,1.90517541785761,24.5507640540487));
#22720=CARTESIAN_POINT('Ctrl Pts',(0.761504884129454,2.30610318635139,24.4435421623461));
#22721=CARTESIAN_POINT('Ctrl Pts',(2.35045883035646,0.611019542610869,24.3324090443546));
#22722=CARTESIAN_POINT('Ctrl Pts',(1.7881803418832,-1.64329323602198,24.2212759263629));
#22723=CARTESIAN_POINT('Ctrl Pts',(-0.410711177573986,-2.39359936565602,
24.1101428083714));
#22724=CARTESIAN_POINT('Ctrl Pts',(-1.87173917948976,-1.23918996178022,
24.0210757394045));
#22725=CARTESIAN_POINT('Ctrl Pts',(-2.05313249987952,-0.278167083222276,
23.9690530431015));
#22726=CARTESIAN_POINT('Ctrl Pts',(-2.05188677382997,-0.00102040058744382,
23.9540747194623));
#22727=CARTESIAN_POINT('Origin',(0.,0.,30.5459252805377));
#22728=CARTESIAN_POINT('',(-2.05557731494487,0.00179379848086081,25.3540747194623));
#22729=CARTESIAN_POINT('',(-2.05258580046671,-0.00147696805610269,25.2959252805377));
#22730=CARTESIAN_POINT('',(-2.05475,1.58232769237955E-13,30.5459252805377));
#22731=CARTESIAN_POINT('Ctrl Pts',(-2.05258580046672,-0.00147696805610264,
25.2959252805377));
#22732=CARTESIAN_POINT('Ctrl Pts',(-2.04962418836947,0.443900223161274,
25.2718344101756));
#22733=CARTESIAN_POINT('Ctrl Pts',(-1.68833128126405,1.57850722809391,25.2106991671496));
#22734=CARTESIAN_POINT('Ctrl Pts',(0.183061725931824,2.4216710176215,25.1125195514598));
#22735=CARTESIAN_POINT('Ctrl Pts',(2.13381500276998,1.15967049071781,25.0013864334682));
#22736=CARTESIAN_POINT('Ctrl Pts',(2.13161680293297,-1.1637061134762,24.8902533154767));
#22737=CARTESIAN_POINT('Ctrl Pts',(0.178479005431905,-2.42201307959068,
24.7791201974851));
#22738=CARTESIAN_POINT('Ctrl Pts',(-1.68997690020491,-1.57591568347207,
24.6810108525055));
#22739=CARTESIAN_POINT('Ctrl Pts',(-2.04963379766141,-0.442630106399392,
24.6199458801896));
#22740=CARTESIAN_POINT('Ctrl Pts',(-2.05255723160113,0.00146350343929682,
24.5959252805377));
#22741=CARTESIAN_POINT('Ctrl Pts',(-2.05557731494487,0.00179379848086123,
25.3540747194623));
#22742=CARTESIAN_POINT('Ctrl Pts',(-2.05678373801941,0.13359791683739,25.3469188484011));
#22743=CARTESIAN_POINT('Ctrl Pts',(-1.98518594980207,0.946417566930667,
25.3027186046759));
#22744=CARTESIAN_POINT('Ctrl Pts',(-0.902106643086596,2.25481821865058,
25.221473988287));
#22745=CARTESIAN_POINT('Ctrl Pts',(1.40506247979517,1.98085865788643,25.1103408702954));
#22746=CARTESIAN_POINT('Ctrl Pts',(2.42626311844678,-0.106060712410309,
24.9992077523039));
#22747=CARTESIAN_POINT('Ctrl Pts',(1.22685225431082,-2.09590914420127,24.8880746343123));
#22748=CARTESIAN_POINT('Ctrl Pts',(-1.09542208140494,-2.16749903303861,
24.7769415163207));
#22749=CARTESIAN_POINT('Ctrl Pts',(-2.0216683440278,-0.825407580955758,
24.6989415447041));
#22750=CARTESIAN_POINT('Ctrl Pts',(-2.0577113705737,-0.0731103635467968,
24.6579859457513));
#22751=CARTESIAN_POINT('Ctrl Pts',(-2.05720656193685,-0.00121771516567365,
24.6540747194623));
#22752=CARTESIAN_POINT('Origin',(0.,0.,30.5459252805377));
#22753=CARTESIAN_POINT('',(-2.05138931231396,9.0883460209662E-5,26.0540747194623));
#22754=CARTESIAN_POINT('',(-2.05788771163865,-0.000632027364112667,25.9959252805377));
#22755=CARTESIAN_POINT('',(-2.05475,1.58232769237955E-13,30.5459252805377));
#22756=CARTESIAN_POINT('Ctrl Pts',(-2.05788771163865,-0.000632027364112779,
25.9959252805377));
#22757=CARTESIAN_POINT('Ctrl Pts',(-2.05527788428679,0.645044426388679,
25.9607673128253));
#22758=CARTESIAN_POINT('Ctrl Pts',(-1.37998469315385,1.97574570518029,25.8885649724492));
#22759=CARTESIAN_POINT('Ctrl Pts',(0.886049547518136,2.26117631167387,25.7793182594091));
#22760=CARTESIAN_POINT('Ctrl Pts',(2.38026485126002,0.482017998562706,25.6681851414176));
#22761=CARTESIAN_POINT('Ctrl Pts',(1.69596807681793,-1.73830215885906,25.557052023426));
#22762=CARTESIAN_POINT('Ctrl Pts',(-0.540545434181373,-2.36765976159588,
25.4459189054345));
#22763=CARTESIAN_POINT('Ctrl Pts',(-1.9047552100369,-1.16335890299012,25.358876657805));
#22764=CARTESIAN_POINT('Ctrl Pts',(-2.0541782397826,-0.240953349974224,
25.3088787828394));
#22765=CARTESIAN_POINT('Ctrl Pts',(-2.05258580046672,-0.00147696805610264,
25.2959252805377));
#22766=CARTESIAN_POINT('Ctrl Pts',(-2.05138931231396,9.08834602098355E-5,
26.0540747194623));
#22767=CARTESIAN_POINT('Ctrl Pts',(-2.05152243725439,0.337478144257027,
26.0358517510509));
#22768=CARTESIAN_POINT('Ctrl Pts',(-1.81315796563237,1.3605424797094,25.9805844099755));
#22769=CARTESIAN_POINT('Ctrl Pts',(-0.200277927177756,2.42030790331167,
25.8882726962363));
#22770=CARTESIAN_POINT('Ctrl Pts',(1.92475392154391,1.48098748682692,25.7771395782448));
#22771=CARTESIAN_POINT('Ctrl Pts',(2.28817522362595,-0.813790968595164,
25.6660064602532));
#22772=CARTESIAN_POINT('Ctrl Pts',(0.557368499380946,-2.36375589911376,
25.5548733422617));
#22773=CARTESIAN_POINT('Ctrl Pts',(-1.53926998825786,-1.78981768810613,
25.4508960953314));
#22774=CARTESIAN_POINT('Ctrl Pts',(-2.05053835075894,-0.548723052508241,
25.3839632210649));
#22775=CARTESIAN_POINT('Ctrl Pts',(-2.05557731494487,0.00179379848086123,
25.3540747194623));
#22776=CARTESIAN_POINT('Origin',(0.,0.,30.5459252805377));
#22777=CARTESIAN_POINT('',(-2.05524375550136,-0.00184130802409817,26.7540747194623));
#22778=CARTESIAN_POINT('',(-2.05444749037063,0.00187707957529171,26.6959252805377));
#22779=CARTESIAN_POINT('',(-2.05475,1.58232769237955E-13,30.5459252805377));
#22780=CARTESIAN_POINT('Ctrl Pts',(-2.05444749037063,0.00187707957529195,
26.6959252805377));
#22781=CARTESIAN_POINT('Ctrl Pts',(-2.05598194935013,0.171214930317575,
26.686744588139));
#22782=CARTESIAN_POINT('Ctrl Pts',(-1.95938878154241,1.02210918950486,26.6405195230765));
#22783=CARTESIAN_POINT('Ctrl Pts',(-0.777884683860044,2.30062981105139,
26.5572500853501));
#22784=CARTESIAN_POINT('Ctrl Pts',(1.51092586075795,1.90134298806969,26.4461169673585));
#22785=CARTESIAN_POINT('Ctrl Pts',(2.4168775880718,-0.238127775426892,26.3349838493669));
#22786=CARTESIAN_POINT('Ctrl Pts',(1.11080781944703,-2.15965462534927,26.2238507313753));
#22787=CARTESIAN_POINT('Ctrl Pts',(-1.21191698652597,-2.10458055943487,
26.1127176133838));
#22788=CARTESIAN_POINT('Ctrl Pts',(-2.04153625209659,-0.750103919255093,
26.0367424631046));
#22789=CARTESIAN_POINT('Ctrl Pts',(-2.05802774223653,-0.0352758745116443,
25.9978116854892));
#22790=CARTESIAN_POINT('Ctrl Pts',(-2.05788771163865,-0.000632027364112779,
25.9959252805377));
#22791=CARTESIAN_POINT('Ctrl Pts',(-2.05524375550136,-0.00184130802409798,
26.7540747194623));
#22792=CARTESIAN_POINT('Ctrl Pts',(-2.05026254246359,0.537878244060909,
26.7247846537006));
#22793=CARTESIAN_POINT('Ctrl Pts',(-1.55589885109608,1.76827887673406,26.6584502152751));
#22794=CARTESIAN_POINT('Ctrl Pts',(0.51920669687721,2.37243040203942,26.5550714041857));
#22795=CARTESIAN_POINT('Ctrl Pts',(2.27476474931693,0.850556836234861,26.4439382861941));
#22796=CARTESIAN_POINT('Ctrl Pts',(1.9483685659561,-1.44977981832677,26.3328051682026));
#22797=CARTESIAN_POINT('Ctrl Pts',(-0.161251214260656,-2.42322092316419,
26.221672050211));
#22798=CARTESIAN_POINT('Ctrl Pts',(-1.8015641250331,-1.38288211781774,26.1287619006309));
#22799=CARTESIAN_POINT('Ctrl Pts',(-2.05125181559754,-0.348376055716531,
26.0728961237147));
#22800=CARTESIAN_POINT('Ctrl Pts',(-2.05138931231396,9.08834602098355E-5,
26.0540747194623));
#22801=CARTESIAN_POINT('Origin',(0.,0.,30.5459252805377));
#22802=CARTESIAN_POINT('',(-2.05744477280677,0.00105931724472513,27.4540747194623));
#22803=CARTESIAN_POINT('',(-2.05150643897842,-0.000517795507161443,27.3959252805377));
#22804=CARTESIAN_POINT('',(-2.05475,1.58232769237955E-13,30.5459252805377));
#22805=CARTESIAN_POINT('Ctrl Pts',(-2.05150643897842,-0.000517795507161516,
27.3959252805377));
#22806=CARTESIAN_POINT('Ctrl Pts',(-2.05066106742218,0.374304485575549,
27.3756774907888));
#22807=CARTESIAN_POINT('Ctrl Pts',(-1.77290985721247,1.4360498631238,27.318385328376));
#22808=CARTESIAN_POINT('Ctrl Pts',(-0.0680801792595378,2.42762578972398,
27.2240487932994));
#22809=CARTESIAN_POINT('Ctrl Pts',(2.00260341844735,1.37389291172196,27.1129156753079));
#22810=CARTESIAN_POINT('Ctrl Pts',(2.24042554204435,-0.937280921003925,
27.0017825573163));
#22811=CARTESIAN_POINT('Ctrl Pts',(0.427722029271838,-2.39061831907088,
26.8906494393248));
#22812=CARTESIAN_POINT('Ctrl Pts',(-1.59436319612448,-1.716657147866,26.7886970137318));
#22813=CARTESIAN_POINT('Ctrl Pts',(-2.04979036076342,-0.512068440541057,
26.7237889608028));
#22814=CARTESIAN_POINT('Ctrl Pts',(-2.05444749037063,0.00187707957529195,
26.6959252805377));
#22815=CARTESIAN_POINT('Ctrl Pts',(-2.05744477280677,0.00105931724472533,
27.4540747194623));
#22816=CARTESIAN_POINT('Ctrl Pts',(-2.05782716792171,0.061933506835561,
27.4507619290143));
#22817=CARTESIAN_POINT('Ctrl Pts',(-2.02776705731346,0.803133697963998,
27.4104047659024));
#22818=CARTESIAN_POINT('Ctrl Pts',(-1.13020663702663,2.14956575456656,27.3330032301266));
#22819=CARTESIAN_POINT('Ctrl Pts',(1.19291950474651,2.1154065927935,27.2218701121351));
#22820=CARTESIAN_POINT('Ctrl Pts',(2.42423908872827,0.145143535993706,27.1107369941435));
#22821=CARTESIAN_POINT('Ctrl Pts',(1.43679947210715,-1.95796032739892,26.999603876152));
#22822=CARTESIAN_POINT('Ctrl Pts',(-0.865655485103571,-2.26906197521519,
26.8884707581604));
#22823=CARTESIAN_POINT('Ctrl Pts',(-1.97780974213485,-0.968776180348794,
26.8066277059305));
#22824=CARTESIAN_POINT('Ctrl Pts',(-2.05656249117625,-0.144727673729697,
26.7618290263645));
#22825=CARTESIAN_POINT('Ctrl Pts',(-2.05524375550136,-0.00184130802409798,
26.7540747194623));
#22826=CARTESIAN_POINT('Origin',(0.,0.,30.5459252805377));
#22827=CARTESIAN_POINT('',(-2.05206134370476,0.00116288414692314,28.1540747194623));
#22828=CARTESIAN_POINT('',(-2.05634566411282,-0.00160712594267666,28.0959252805377));
#22829=CARTESIAN_POINT('',(-2.05475,1.58232769237955E-13,30.5459252805377));
#22830=CARTESIAN_POINT('Ctrl Pts',(-2.05634566411282,-0.00160712594267667,
28.0959252805377));
#22831=CARTESIAN_POINT('Ctrl Pts',(-2.05139599927139,0.574624822876943,
28.0646103934386));
#22832=CARTESIAN_POINT('Ctrl Pts',(-1.49844858220422,1.84084696248835,27.9962511336756));
#22833=CARTESIAN_POINT('Ctrl Pts',(0.647725970766636,2.34060717669366,27.8908475012488));
#22834=CARTESIAN_POINT('Ctrl Pts',(2.31773743276476,0.725325684108574,27.7797143832572));
#22835=CARTESIAN_POINT('Ctrl Pts',(1.86646417683138,-1.55380676849557,27.6685812652656));
#22836=CARTESIAN_POINT('Ctrl Pts',(-0.293070456042677,-2.41083184926652,
27.5574481472741));
#22837=CARTESIAN_POINT('Ctrl Pts',(-1.83979104753125,-1.30723380638585,
27.4665628190314));
#22838=CARTESIAN_POINT('Ctrl Pts',(-2.05220771816071,-0.311452154301391,
27.4127218634526));
#22839=CARTESIAN_POINT('Ctrl Pts',(-2.05150643897842,-0.000517795507161516,
27.3959252805377));
#22840=CARTESIAN_POINT('Ctrl Pts',(-2.05206134370476,0.00116288414692349,
28.1540747194623));
#22841=CARTESIAN_POINT('Ctrl Pts',(-2.05344175345948,0.26718383829129,28.1396948316641));
#22842=CARTESIAN_POINT('Ctrl Pts',(-1.8817859926555,1.21680050673287,28.0882705712019));
#22843=CARTESIAN_POINT('Ctrl Pts',(-0.449219217968869,2.38665611117453,
27.999801938076));
#22844=CARTESIAN_POINT('Ctrl Pts',(1.76146356868064,1.6719019509933,27.8886688200844));
#22845=CARTESIAN_POINT('Ctrl Pts',(2.36000201199169,-0.573068912759941,
27.7775357020928));
#22846=CARTESIAN_POINT('Ctrl Pts',(0.798565170672349,-2.29353090612058,
27.6664025841013));
#22847=CARTESIAN_POINT('Ctrl Pts',(-1.42541352622956,-1.92615781520145,
27.5585822565578));
#22848=CARTESIAN_POINT('Ctrl Pts',(-2.05355113918859,-0.618775460476319,
27.4878063016781));
#22849=CARTESIAN_POINT('Ctrl Pts',(-2.05744477280677,0.00105931724472533,
27.4540747194623));
#22850=CARTESIAN_POINT('Origin',(0.,0.,30.5459252805377));
#22851=CARTESIAN_POINT('',(-2.05269153525815,-0.00250469671298922,28.8540747194623));
#22852=CARTESIAN_POINT('',(-2.05654741388298,0.00148211099959903,28.7959252805377));
#22853=CARTESIAN_POINT('',(-2.05475,1.58232769237955E-13,30.5459252805377));
#22854=CARTESIAN_POINT('',(-0.530170217188662,-1.98517432567171,29.));
#22855=CARTESIAN_POINT('Ctrl Pts',(-0.530170217188634,-1.98517432567172,
29.));
#22856=CARTESIAN_POINT('Ctrl Pts',(-1.19025956241812,-1.80888768575368,
28.9629556273361));
#22857=CARTESIAN_POINT('Ctrl Pts',(-1.92498012557237,-1.11310439800918,
28.9143138671569));
#22858=CARTESIAN_POINT('Ctrl Pts',(-2.05431617558531,-0.216806977145675,
28.8656721069777));
#22859=CARTESIAN_POINT('Ctrl Pts',(-2.05269153525815,-0.00250469671298928,
28.8540747194623));
#22860=CARTESIAN_POINT('',(0.531258132123393,-1.9887550962016,29.));
#22861=CARTESIAN_POINT('Origin',(0.,0.,29.));
#22862=CARTESIAN_POINT('Ctrl Pts',(0.53125844574167,-1.98875612844696,29.));
#22863=CARTESIAN_POINT('Ctrl Pts',(-0.113293144729996,-2.16008022379809,
28.9636818543909));
#22864=CARTESIAN_POINT('Ctrl Pts',(-1.49287139477788,-1.84060537719605,
28.8956569479035));
#22865=CARTESIAN_POINT('Ctrl Pts',(-2.05167852337285,-0.581660892242976,
28.8276320414161));
#22866=CARTESIAN_POINT('Ctrl Pts',(-2.05654741388298,0.00148211099959938,
28.7959252805377));
#22867=CARTESIAN_POINT('Origin',(-4.61329551933804E-17,0.,18.));
#22868=CARTESIAN_POINT('Ctrl Pts',(-0.76990204067047,-1.47743251885541,
18.));
#22869=CARTESIAN_POINT('Ctrl Pts',(-0.718150631325321,-1.51251203856552,
18.));
#22870=CARTESIAN_POINT('Ctrl Pts',(-0.664423318055599,-1.5443372549372,
18.));
#22871=CARTESIAN_POINT('Ctrl Pts',(-0.609051292693035,-1.57297177961208,
18.));
#22872=CARTESIAN_POINT('Ctrl Pts',(-0.5739254652649,-1.59113639189834,18.));
#22873=CARTESIAN_POINT('Ctrl Pts',(-0.538136890245182,-1.60801638025237,
18.));
#22874=CARTESIAN_POINT('Ctrl Pts',(-0.501762501547232,-1.62362076387509,
18.));
#22875=CARTESIAN_POINT('Ctrl Pts',(-0.476746252182073,-1.63435257727097,
18.));
#22876=CARTESIAN_POINT('Ctrl Pts',(-0.45145279912961,-1.64448092345754,
18.));
#22877=CARTESIAN_POINT('Ctrl Pts',(-0.425905888015268,-1.65400710125167,
18.));
#22878=CARTESIAN_POINT('Ctrl Pts',(-0.41253154468577,-1.65899425495751,
18.));
#22879=CARTESIAN_POINT('Ctrl Pts',(-0.399088138260695,-1.66381606897088,
18.));
#22880=CARTESIAN_POINT('Ctrl Pts',(-0.385592178738817,-1.66846843086131,
18.));
#22881=CARTESIAN_POINT('Ctrl Pts',(-0.323215765718591,-1.68997098844724,
18.));
#22882=CARTESIAN_POINT('Ctrl Pts',(-0.259649271127304,-1.70788387774854,
18.));
#22883=CARTESIAN_POINT('Ctrl Pts',(-0.195242368079891,-1.72225306016113,
18.));
#22884=CARTESIAN_POINT('Ctrl Pts',(-0.148812097770522,-1.73261165515598,
18.));
#22885=CARTESIAN_POINT('Ctrl Pts',(-0.101944183746803,-1.74112782318747,
18.));
#22886=CARTESIAN_POINT('Ctrl Pts',(-0.0547605417505049,-1.7478047767719,
18.));
#22887=CARTESIAN_POINT('Ctrl Pts',(-0.0416678989315785,-1.7496575156598,
18.));
#22888=CARTESIAN_POINT('Ctrl Pts',(-0.0285509121040071,-1.75136856900838,
18.));
#22889=CARTESIAN_POINT('Ctrl Pts',(-0.0154121163252258,-1.75293783687761,
18.));
#22890=CARTESIAN_POINT('Ctrl Pts',(-0.00237504775858612,-1.75449495468012,
18.));
#22891=CARTESIAN_POINT('Ctrl Pts',(0.0106749433642533,-1.75591142474928,
18.));
#22892=CARTESIAN_POINT('Ctrl Pts',(0.0237314174192055,-1.75718732825168,
18.));
#22893=CARTESIAN_POINT('Ctrl Pts',(0.091264839179258,-1.76378682280057,
18.));
#22894=CARTESIAN_POINT('Ctrl Pts',(0.159001654673738,-1.76663304455511,
18.));
#22895=CARTESIAN_POINT('Ctrl Pts',(0.226587398060141,-1.76577341924289,
18.));
#22896=CARTESIAN_POINT('Ctrl Pts',(0.295141384080251,-1.7649014788205,18.));
#22897=CARTESIAN_POINT('Ctrl Pts',(0.363540948302614,-1.76021708355991,
18.));
#22898=CARTESIAN_POINT('Ctrl Pts',(0.431437640562689,-1.75172144275485,
18.));
#22899=CARTESIAN_POINT('Ctrl Pts',(0.473486932876576,-1.74645998344492,
18.));
#22900=CARTESIAN_POINT('Ctrl Pts',(0.51534371614305,-1.73973575700245,18.));
#22901=CARTESIAN_POINT('Ctrl Pts',(0.556926593833155,-1.73153911679675,
18.));
#22902=CARTESIAN_POINT('Ctrl Pts',(0.591007346597968,-1.72482126358721,
18.));
#22903=CARTESIAN_POINT('Ctrl Pts',(0.624904151165585,-1.71711422326624,
18.));
#22904=CARTESIAN_POINT('Ctrl Pts',(0.658571851627645,-1.70840869390865,
18.));
#22905=CARTESIAN_POINT('Ctrl Pts',(0.672311891199144,-1.70485590247287,
18.));
#22906=CARTESIAN_POINT('Ctrl Pts',(0.686016147209164,-1.70113595255256,
18.));
#22907=CARTESIAN_POINT('Ctrl Pts',(0.699658483569614,-1.69725500100484,
18.));
#22908=CARTESIAN_POINT('Ctrl Pts',(0.767448475183213,-1.67797020506366,
18.));
#22909=CARTESIAN_POINT('Ctrl Pts',(0.833829915647279,-1.65468448734625,
18.));
#22910=CARTESIAN_POINT('Ctrl Pts',(0.898440425741411,-1.62741601672657,
18.));
#22911=CARTESIAN_POINT('Ctrl Pts',(0.905588436264334,-1.62439924260346,
18.));
#22912=CARTESIAN_POINT('Ctrl Pts',(0.912714779380887,-1.62133366961292,
18.));
#22913=CARTESIAN_POINT('Ctrl Pts',(0.919818968510682,-1.61821928330016,
18.));
#22914=CARTESIAN_POINT('Ctrl Pts',(0.981562897597664,-1.5911515287498,18.));
#22915=CARTESIAN_POINT('Ctrl Pts',(1.04163420093584,-1.56040088867233,18.));
#22916=CARTESIAN_POINT('Ctrl Pts',(1.09989073176884,-1.52627787643936,18.));
#22917=CARTESIAN_POINT('Ctrl Pts',(1.16256978924498,-1.48956442621451,18.));
#22918=CARTESIAN_POINT('Ctrl Pts',(1.22314908610384,-1.44894713491801,18.));
#22919=CARTESIAN_POINT('Ctrl Pts',(1.28143172127969,-1.40475162384861,18.));
#22920=CARTESIAN_POINT('Ctrl Pts',(1.29192404292766,-1.3967953343614,18.));
#22921=CARTESIAN_POINT('Ctrl Pts',(1.30234185924819,-1.38872293100869,18.));
#22922=CARTESIAN_POINT('Ctrl Pts',(1.31268391753456,-1.38053612650623,18.));
#22923=CARTESIAN_POINT('Ctrl Pts',(1.32189334531869,-1.37324591572222,18.));
#22924=CARTESIAN_POINT('Ctrl Pts',(1.33103577871284,-1.36587044480612,18.));
#22925=CARTESIAN_POINT('Ctrl Pts',(1.34010835513525,-1.35841319152643,18.));
#22926=CARTESIAN_POINT('Ctrl Pts',(1.39501139656529,-1.31328533955731,18.));
#22927=CARTESIAN_POINT('Ctrl Pts',(1.44738363710458,-1.26514600652793,18.));
#22928=CARTESIAN_POINT('Ctrl Pts',(1.49707481635619,-1.21434556759909,18.));
#22929=CARTESIAN_POINT('Ctrl Pts',(1.54781663370407,-1.16247103710612,18.));
#22930=CARTESIAN_POINT('Ctrl Pts',(1.59576358322206,-1.10782114035041,18.));
#22931=CARTESIAN_POINT('Ctrl Pts',(1.64073548547958,-1.0507176415564,18.));
#22932=CARTESIAN_POINT('Ctrl Pts',(1.68598205390614,-0.993265382793032,
18.));
#22933=CARTESIAN_POINT('Ctrl Pts',(1.72821791230343,-0.933328730063129,
18.));
#22934=CARTESIAN_POINT('Ctrl Pts',(1.76722761838473,-0.871193823462839,
18.));
#22935=CARTESIAN_POINT('Ctrl Pts',(1.7768492490117,-0.85586842933904,18.));
#22936=CARTESIAN_POINT('Ctrl Pts',(1.78627443371382,-0.840409138082932,
18.));
#22937=CARTESIAN_POINT('Ctrl Pts',(1.79549955621922,-0.824819938514783,
18.));
#22938=CARTESIAN_POINT('Ctrl Pts',(1.80276226427272,-0.812546951875862,
18.));
#22939=CARTESIAN_POINT('Ctrl Pts',(1.80990173580295,-0.800191855082187,
18.));
#22940=CARTESIAN_POINT('Ctrl Pts',(1.81690568883513,-0.787775762904653,
18.));
#22941=CARTESIAN_POINT('Ctrl Pts',(1.85392851007218,-0.722144431706478,
18.));
#22942=CARTESIAN_POINT('Ctrl Pts',(1.8872372067062,-0.654696535289144,18.));
#22943=CARTESIAN_POINT('Ctrl Pts',(1.91665075707102,-0.585778873556434,
18.));
#22944=CARTESIAN_POINT('Ctrl Pts',(1.94609703420479,-0.516784531097881,
18.));
#22945=CARTESIAN_POINT('Ctrl Pts',(1.97164025822083,-0.446316320651974,
18.));
#22946=CARTESIAN_POINT('Ctrl Pts',(1.99306307145695,-0.374684480774626,
18.));
#22947=CARTESIAN_POINT('Ctrl Pts',(2.01399797892016,-0.304684060067817,
18.));
#22948=CARTESIAN_POINT('Ctrl Pts',(2.03099858110164,-0.233571531454558,
18.));
#22949=CARTESIAN_POINT('Ctrl Pts',(2.04381843104347,-0.161613213448295,
18.));
#22950=CARTESIAN_POINT('Ctrl Pts',(2.0465707882259,-0.146164125175105,18.));
#22951=CARTESIAN_POINT('Ctrl Pts',(2.04913025745793,-0.130675991664333,
18.));
#22952=CARTESIAN_POINT('Ctrl Pts',(2.05149409115388,-0.115151364067968,
18.));
#22953=CARTESIAN_POINT('Ctrl Pts',(2.05350777753846,-0.101926351128162,
18.));
#22954=CARTESIAN_POINT('Ctrl Pts',(2.05537949127336,-0.0886748543274951,
18.));
#22955=CARTESIAN_POINT('Ctrl Pts',(2.0571100610898,-0.075398570255039,18.));
#22956=CARTESIAN_POINT('Ctrl Pts',(1.81742788875943,0.958620587959298,18.));
#22957=CARTESIAN_POINT('Ctrl Pts',(1.77657712986193,1.02110689942424,18.));
#22958=CARTESIAN_POINT('Ctrl Pts',(1.7321315874396,1.08104302965111,18.));
#22959=CARTESIAN_POINT('Ctrl Pts',(1.68441962095058,1.13827891073254,18.));
#22960=CARTESIAN_POINT('Ctrl Pts',(1.63796461382492,1.19400692739462,18.));
#22961=CARTESIAN_POINT('Ctrl Pts',(1.58841202635459,1.24717530230443,18.));
#22962=CARTESIAN_POINT('Ctrl Pts',(1.5360388941578,1.29760785240109,18.));
#22963=CARTESIAN_POINT('Ctrl Pts',(1.52434810361592,1.3088654639844,18.));
#22964=CARTESIAN_POINT('Ctrl Pts',(1.51251510017348,1.3199880593865,18.));
#22965=CARTESIAN_POINT('Ctrl Pts',(1.50054796988442,1.33096871964239,18.));
#22966=CARTESIAN_POINT('Ctrl Pts',(1.44563515565536,1.38135498119215,18.));
#22967=CARTESIAN_POINT('Ctrl Pts',(1.38801000276354,1.42865729042352,18.));
#22968=CARTESIAN_POINT('Ctrl Pts',(1.32798805944486,1.47270290942279,18.));
#22969=CARTESIAN_POINT('Ctrl Pts',(1.28585164904722,1.5036236723264,18.));
#22970=CARTESIAN_POINT('Ctrl Pts',(1.24253335224023,1.53293855420436,18.));
#22971=CARTESIAN_POINT('Ctrl Pts',(1.19813701502426,1.56057339033618,18.));
#22972=CARTESIAN_POINT('Ctrl Pts',(1.18125759993015,1.57108011002022,18.));
#22973=CARTESIAN_POINT('Ctrl Pts',(1.16422232469794,1.58134384847995,18.));
#22974=CARTESIAN_POINT('Ctrl Pts',(1.14703682092037,1.59136004184456,18.));
#22975=CARTESIAN_POINT('Ctrl Pts',(1.13066871649995,1.60089983194957,18.));
#22976=CARTESIAN_POINT('Ctrl Pts',(1.11415903455404,1.61021779338036,18.));
#22977=CARTESIAN_POINT('Ctrl Pts',(1.09754217891543,1.61929409944754,18.));
#22978=CARTESIAN_POINT('Ctrl Pts',(1.03383800288656,1.65409000861173,18.));
#22979=CARTESIAN_POINT('Ctrl Pts',(0.96849489309373,1.68537885814686,18.));
#22980=CARTESIAN_POINT('Ctrl Pts',(0.901803973692338,1.71299878952967,18.));
#22981=CARTESIAN_POINT('Ctrl Pts',(0.836547032382178,1.74002484131329,18.));
#22982=CARTESIAN_POINT('Ctrl Pts',(0.769998695925455,1.76353820983274,18.));
#22983=CARTESIAN_POINT('Ctrl Pts',(0.702423095374045,1.78333899888662,18.));
#22984=CARTESIAN_POINT('Ctrl Pts',(0.63632849633975,1.8027058295533,18.));
#22985=CARTESIAN_POINT('Ctrl Pts',(0.569250406487646,1.81852114051121,18.));
#22986=CARTESIAN_POINT('Ctrl Pts',(0.501439873296343,1.83054930271628,18.));
#22987=CARTESIAN_POINT('Ctrl Pts',(0.479368946632993,1.83446422084816,18.));
#22988=CARTESIAN_POINT('Ctrl Pts',(0.457220505887409,1.83797754309986,18.));
#22989=CARTESIAN_POINT('Ctrl Pts',(0.435003501016378,1.8410799689604,18.));
#22990=CARTESIAN_POINT('Ctrl Pts',(0.422525526393832,1.84282241765593,18.));
#22991=CARTESIAN_POINT('Ctrl Pts',(0.410024644591693,1.8444352959301,18.));
#22992=CARTESIAN_POINT('Ctrl Pts',(0.397520124711553,1.84591507854722,18.));
#22993=CARTESIAN_POINT('Ctrl Pts',(0.329697086251002,1.85394124463088,18.));
#22994=CARTESIAN_POINT('Ctrl Pts',(0.261648673649785,1.85807376866092,18.));
#22995=CARTESIAN_POINT('Ctrl Pts',(0.193620068644232,1.85813442656068,18.));
#22996=CARTESIAN_POINT('Ctrl Pts',(0.183819205913209,1.8581431655279,18.));
#22997=CARTESIAN_POINT('Ctrl Pts',(0.174018760470502,1.85806730026065,18.));
#22998=CARTESIAN_POINT('Ctrl Pts',(0.164219474866952,1.85790620769987,18.));
#22999=CARTESIAN_POINT('Ctrl Pts',(0.0948546883628424,1.85676590507598,
18.));
#23000=CARTESIAN_POINT('Ctrl Pts',(0.0255465610762253,1.85135924381112,
18.));
#23001=CARTESIAN_POINT('Ctrl Pts',(-0.0433793899519713,1.84185967358528,
18.));
#23002=CARTESIAN_POINT('Ctrl Pts',(-0.107679490493548,1.83299765120457,
18.));
#23003=CARTESIAN_POINT('Ctrl Pts',(-0.171647506113411,1.82057273856315,
18.));
#23004=CARTESIAN_POINT('Ctrl Pts',(-0.234998654721344,1.80469130867306,
18.));
#23005=CARTESIAN_POINT('Ctrl Pts',(-0.248859420949268,1.80121656840538,
18.));
#23006=CARTESIAN_POINT('Ctrl Pts',(-0.262690559254527,1.79757625312175,
18.));
#23007=CARTESIAN_POINT('Ctrl Pts',(-0.276488909329196,1.79377129906237,
18.));
#23008=CARTESIAN_POINT('Ctrl Pts',(-0.287551928784525,1.79072062412242,
18.));
#23009=CARTESIAN_POINT('Ctrl Pts',(-0.298593335771869,1.7875641728674,18.));
#23010=CARTESIAN_POINT('Ctrl Pts',(-0.309598430415198,1.78430655809845,
18.));
#23011=CARTESIAN_POINT('Ctrl Pts',(-0.375170595375803,1.7648965611897,18.));
#23012=CARTESIAN_POINT('Ctrl Pts',(-0.439577642441152,1.74186598076745,
18.));
#23013=CARTESIAN_POINT('Ctrl Pts',(-0.502516607245069,1.7153970604683,18.));
#23014=CARTESIAN_POINT('Ctrl Pts',(-0.565162708177599,1.68905130378479,
18.));
#23015=CARTESIAN_POINT('Ctrl Pts',(-0.626355250869692,1.65929842798695,
18.));
#23016=CARTESIAN_POINT('Ctrl Pts',(-0.685765693704282,1.62627659429092,
18.));
#23017=CARTESIAN_POINT('Ctrl Pts',(-0.743900118729632,1.59396400371579,
18.));
#23018=CARTESIAN_POINT('Ctrl Pts',(-0.800328846584056,1.55852066563614,
18.));
#23019=CARTESIAN_POINT('Ctrl Pts',(-0.854704114065593,1.52004664194688,
18.));
#23020=CARTESIAN_POINT('Ctrl Pts',(-0.866188890450393,1.511920418773,18.));
#23021=CARTESIAN_POINT('Ctrl Pts',(-0.877581894981679,1.50365890819555,
18.));
#23022=CARTESIAN_POINT('Ctrl Pts',(-0.888879573567156,1.49526292491495,
18.));
#23023=CARTESIAN_POINT('Ctrl Pts',(-0.899528318420504,1.48734920325332,
18.));
#23024=CARTESIAN_POINT('Ctrl Pts',(-0.910093638757256,1.47931487609194,
18.));
#23025=CARTESIAN_POINT('Ctrl Pts',(-0.92055590532325,1.47117394178587,18.));
#23026=CARTESIAN_POINT('Ctrl Pts',(-0.972133500375775,1.43104020878076,
18.));
#23027=CARTESIAN_POINT('Ctrl Pts',(-1.02130427170992,1.38824940731442,18.));
#23028=CARTESIAN_POINT('Ctrl Pts',(-1.06777672763296,1.34293373535765,18.));
#23029=CARTESIAN_POINT('Ctrl Pts',(-1.11336328516427,1.29848191017009,18.));
#23030=CARTESIAN_POINT('Ctrl Pts',(-1.15635400485184,1.25159989688763,18.));
#23031=CARTESIAN_POINT('Ctrl Pts',(-1.19643122999363,1.20238672968345,18.));
#23032=CARTESIAN_POINT('Ctrl Pts',(-1.23520491944242,1.15477425014636,18.));
#23033=CARTESIAN_POINT('Ctrl Pts',(-1.27125189947612,1.10497922195428,18.));
#23034=CARTESIAN_POINT('Ctrl Pts',(-1.30423784606576,1.05307598279351,18.));
#23035=CARTESIAN_POINT('Ctrl Pts',(-1.30970514760245,1.0444732083225,18.));
#23036=CARTESIAN_POINT('Ctrl Pts',(-1.31508824330323,1.03581249296888,18.));
#23037=CARTESIAN_POINT('Ctrl Pts',(-1.32038547188529,1.02709414911752,18.));
#23038=CARTESIAN_POINT('Ctrl Pts',(-1.32604175486339,1.01778486235373,18.));
#23039=CARTESIAN_POINT('Ctrl Pts',(-1.33160013514927,1.00840986902262,18.));
#23040=CARTESIAN_POINT('Ctrl Pts',(-1.33706021092902,0.998970828965279,
18.));
#23041=CARTESIAN_POINT('Origin',(0.,0.,30.5459252805377));
#23042=CARTESIAN_POINT('Ctrl Pts',(-2.05654741388298,0.0014821109995993,
28.7959252805377));
#23043=CARTESIAN_POINT('Ctrl Pts',(-2.05736705760088,0.0996501635064194,
28.7905876687522));
#23044=CARTESIAN_POINT('Ctrl Pts',(-2.00636102311651,0.87830624679129,28.7482056843029));
#23045=CARTESIAN_POINT('Ctrl Pts',(-1.01137155273683,2.20819495159188,28.6687793271897));
#23046=CARTESIAN_POINT('Ctrl Pts',(1.30642536602,2.04713238573498,28.5576462091981));
#23047=CARTESIAN_POINT('Ctrl Pts',(2.428549244938,0.0128757876891458,28.4465130912066));
#23048=CARTESIAN_POINT('Ctrl Pts',(1.32795945590719,-2.03338475909482,28.335379973215));
#23049=CARTESIAN_POINT('Ctrl Pts',(-0.988025992283097,-2.21849736833443,
28.2242468552234));
#23050=CARTESIAN_POINT('Ctrl Pts',(-2.00194536412696,-0.89317403920961,
28.144428624331));
#23051=CARTESIAN_POINT('Ctrl Pts',(-2.05725127278289,-0.107036617744751,
28.1016547661024));
#23052=CARTESIAN_POINT('Ctrl Pts',(-2.05634566411282,-0.00160712594267667,
28.0959252805377));
#23053=CARTESIAN_POINT('Ctrl Pts',(-2.05269153525815,-0.00250469671298928,
28.8540747194623));
#23054=CARTESIAN_POINT('Ctrl Pts',(-2.04912674980779,0.46771732011864,28.8286277343138));
#23055=CARTESIAN_POINT('Ctrl Pts',(-1.65657263400563,1.62959319222768,28.7661363765015));
#23056=CARTESIAN_POINT('Ctrl Pts',(0.271806531570387,2.41264813750898,28.6666006460253));
#23057=CARTESIAN_POINT('Ctrl Pts',(2.17449559304179,1.08136903079269,28.5554675280338));
#23058=CARTESIAN_POINT('Ctrl Pts',(2.08783197155072,-1.24094928383581,28.4443344100422));
#23059=CARTESIAN_POINT('Ctrl Pts',(0.0898704340492965,-2.42681281153263,
28.3332012920506));
#23060=CARTESIAN_POINT('Ctrl Pts',(-1.72098255593206,-1.52582831451086,
28.2364480618574));
#23061=CARTESIAN_POINT('Ctrl Pts',(-2.0498856468959,-0.418119100088083,
28.1767392043279));
#23062=CARTESIAN_POINT('Ctrl Pts',(-2.05206134370476,0.00116288414692349,
28.1540747194623));
#23063=CARTESIAN_POINT('Ctrl Pts',(1.26907087985237,1.07935865304853,29.));
#23064=CARTESIAN_POINT('Ctrl Pts',(1.62796789828802,0.657380514756762,28.9629556273361));
#23065=CARTESIAN_POINT('Ctrl Pts',(1.8855124744847,-0.565459156385445,28.8888668820085));
#23066=CARTESIAN_POINT('Ctrl Pts',(0.545109031726074,-1.89347865825101,
28.7777337640169));
#23067=CARTESIAN_POINT('Ctrl Pts',(-1.29391589325212,-1.48358117411062,
28.6666006460253));
#23068=CARTESIAN_POINT('Ctrl Pts',(-1.94881484284809,0.281688560316987,
28.5554675280338));
#23069=CARTESIAN_POINT('Ctrl Pts',(-0.820024337198962,1.7904138164507,28.4443344100422));
#23070=CARTESIAN_POINT('Ctrl Pts',(1.05925521829386,1.65982360610024,28.3332012920507));
#23071=CARTESIAN_POINT('Ctrl Pts',(1.96907801049602,0.0104397431756257,
28.2220681740591));
#23072=CARTESIAN_POINT('Ctrl Pts',(1.07671514955171,-1.64867697221169,28.1109350560675));
#23073=CARTESIAN_POINT('Ctrl Pts',(-0.801095657935827,-1.79876705956693,
27.999801938076));
#23074=CARTESIAN_POINT('Ctrl Pts',(-1.94571434032061,-0.302602882372122,
27.8886688200844));
#23075=CARTESIAN_POINT('Ctrl Pts',(-1.30953755668062,1.47054040479727,27.7775357020928));
#23076=CARTESIAN_POINT('Ctrl Pts',(0.525178959628771,1.89777420920873,27.6664025841013));
#23077=CARTESIAN_POINT('Ctrl Pts',(1.87923132399858,0.588097135770716,27.5552694661097));
#23078=CARTESIAN_POINT('Ctrl Pts',(1.51333705735544,-1.25983310685661,27.4441363481182));
#23079=CARTESIAN_POINT('Ctrl Pts',(-0.237622766646598,-1.95471267106851,
27.3330032301266));
#23080=CARTESIAN_POINT('Ctrl Pts',(-1.771100924469,-0.860563215060856,27.2218701121351));
#23081=CARTESIAN_POINT('Ctrl Pts',(-1.68359778420962,1.02120806251476,27.1107369941435));
#23082=CARTESIAN_POINT('Ctrl Pts',(-0.0551996976013584,1.96832926909851,
26.9996038761519));
#23083=CARTESIAN_POINT('Ctrl Pts',(1.6237193308837,1.11395819001279,26.8884707581604));
#23084=CARTESIAN_POINT('Ctrl Pts',(1.81654651565683,-0.759951339283385,
26.7773376401688));
#23085=CARTESIAN_POINT('Ctrl Pts',(0.346798832347918,-1.93832345519995,
26.6662045221773));
#23086=CARTESIAN_POINT('Ctrl Pts',(-1.44035279303805,-1.34266567211626,
26.5550714041857));
#23087=CARTESIAN_POINT('Ctrl Pts',(-1.90923685006354,0.481852590706729,
26.4439382861942));
#23088=CARTESIAN_POINT('Ctrl Pts',(-0.630712195308838,1.86536039187814,
26.3328051682025));
#23089=CARTESIAN_POINT('Ctrl Pts',(1.22506508530125,1.54161694518754,26.2216720502111));
#23090=CARTESIAN_POINT('Ctrl Pts',(1.95961458169004,-0.193075008570971,
26.1105389322195));
#23091=CARTESIAN_POINT('Ctrl Pts',(0.900647683269863,-1.75105711440899,
25.9994058142279));
#23092=CARTESIAN_POINT('Ctrl Pts',(-0.982627424042958,-1.70640282857695,
25.8882726962363));
#23093=CARTESIAN_POINT('Ctrl Pts',(-1.96656323702446,-0.0999815104761928,
25.7771395782448));
#23094=CARTESIAN_POINT('Ctrl Pts',(-1.15062297231094,1.59794682114526,25.6660064602532));
#23095=CARTESIAN_POINT('Ctrl Pts',(0.718412724742773,1.83337132753311,25.5548733422617));
#23096=CARTESIAN_POINT('Ctrl Pts',(1.92992881966137,0.390822234143067,25.4437402242701));
#23097=CARTESIAN_POINT('Ctrl Pts',(1.3750980975684,-1.40942275053374,25.3326071062786));
#23098=CARTESIAN_POINT('Ctrl Pts',(-0.438276526753214,-1.91970855959058,
25.221473988287));
#23099=CARTESIAN_POINT('Ctrl Pts',(-1.85052322339412,-0.673001535913663,
25.1103408702954));
#23100=CARTESIAN_POINT('Ctrl Pts',(-1.5690982301005,1.18966298251176,24.9992077523039));
#23101=CARTESIAN_POINT('Ctrl Pts',(0.148427222485663,1.96350111466476,24.8880746343123));
#23102=CARTESIAN_POINT('Ctrl Pts',(1.73010623901437,0.940265744025244,24.7769415163208));
#23103=CARTESIAN_POINT('Ctrl Pts',(1.72832392927915,-0.943537844044948,
24.6658083983292));
#23104=CARTESIAN_POINT('Ctrl Pts',(0.144711533300673,-1.96377845995769,
24.5546752803376));
#23105=CARTESIAN_POINT('Ctrl Pts',(-1.57134655374502,-1.1866917357501,24.4435421623461));
#23106=CARTESIAN_POINT('Ctrl Pts',(-1.8492464272056,0.676501972747513,24.3324090443545));
#23107=CARTESIAN_POINT('Ctrl Pts',(-0.434643184857508,1.92053444892845,
24.221275926363));
#23108=CARTESIAN_POINT('Ctrl Pts',(1.37776260766122,1.40681820595075,24.1101428083714));
#23109=CARTESIAN_POINT('Ctrl Pts',(1.9291858334406,-0.394473430938072,23.9990096903799));
#23110=CARTESIAN_POINT('Ctrl Pts',(0.714942252440661,-1.83472745750944,
23.8878765723883));
#23111=CARTESIAN_POINT('Ctrl Pts',(-1.15364461784582,-1.59576670079913,
23.7767434543968));
#23112=CARTESIAN_POINT('Ctrl Pts',(-1.96637052687012,0.103702549247829,
23.6656103364051));
#23113=CARTESIAN_POINT('Ctrl Pts',(-0.979396734113147,1.70825914453061,
23.5544772184136));
#23114=CARTESIAN_POINT('Ctrl Pts',(0.903959498383989,1.74934973431425,23.443344100422));
#23115=CARTESIAN_POINT('Ctrl Pts',(1.95997641846095,0.189366593518892,23.3322109824305));
#23116=CARTESIAN_POINT('Ctrl Pts',(1.22214577644235,-1.54393230706145,23.2210778644389));
#23117=CARTESIAN_POINT('Ctrl Pts',(-0.634240783365302,-1.86416359163571,
23.1099447464473));
#23118=CARTESIAN_POINT('Ctrl Pts',(-1.91014521476306,-0.478238984380987,
22.9988116284558));
#23119=CARTESIAN_POINT('Ctrl Pts',(-1.43780956302664,1.34538876468221,22.8876785104642));
#23120=CARTESIAN_POINT('Ctrl Pts',(0.350465992424694,1.93766376232249,22.7765453924727));
#23121=CARTESIAN_POINT('Ctrl Pts',(1.8179812774019,0.756512618982733,22.6654122744811));
#23122=CARTESIAN_POINT('Ctrl Pts',(1.6216085422551,-1.11702864929655,22.5542791564896));
#23123=CARTESIAN_POINT('Ctrl Pts',(-0.0589241566538478,-1.96822133192042,
22.443146038498));
#23124=CARTESIAN_POINT('Ctrl Pts',(-1.68552714816096,-1.01802038313401,
22.3320129205065));
#23125=CARTESIAN_POINT('Ctrl Pts',(-1.76946935196913,0.863912889188492,
22.2208798025149));
#23126=CARTESIAN_POINT('Ctrl Pts',(-0.233923559220051,1.95515908204568,
22.1097466845233));
#23127=CARTESIAN_POINT('Ctrl Pts',(1.51571828206865,1.25696672870313,21.9986135665318));
#23128=CARTESIAN_POINT('Ctrl Pts',(1.87811509351815,-0.591651048476953,
21.8874804485402));
#23129=CARTESIAN_POINT('Ctrl Pts',(0.521587049489592,-1.89876649893241,
21.7763473305487));
#23130=CARTESIAN_POINT('Ctrl Pts',(-1.31231799169707,-1.46805611484414,
21.6652142125571));
#23131=CARTESIAN_POINT('Ctrl Pts',(-1.94513795455165,0.306277007675757,
21.5540810945656));
#23132=CARTESIAN_POINT('Ctrl Pts',(-0.797691101513079,1.80029335782399,
21.442947976574));
#23133=CARTESIAN_POINT('Ctrl Pts',(1.07983404443909,1.64661036803806,21.3318148585824));
#23134=CARTESIAN_POINT('Ctrl Pts',(1.9690525710802,-0.0141152405335317,
21.2206817405909));
#23135=CARTESIAN_POINT('Ctrl Pts',(1.05611668348891,-1.66192202538936,21.1095486225993));
#23136=CARTESIAN_POINT('Ctrl Pts',(-0.823418761129365,-1.78867236001269,
20.9984155046078));
#23137=CARTESIAN_POINT('Ctrl Pts',(-1.9493289462109,-0.278359349261021,
20.8872823866162));
#23138=CARTESIAN_POINT('Ctrl Pts',(-1.29113655469699,1.48671909398746,20.7761492686246));
#23139=CARTESIAN_POINT('Ctrl Pts',(0.548754829962253,1.89109370584855,20.6650161506331));
#23140=CARTESIAN_POINT('Ctrl Pts',(1.886404196139,0.564664925157129,20.5538830326415));
#23141=CARTESIAN_POINT('Ctrl Pts',(1.49754219255897,-1.27856741957737,20.4427499146499));
#23142=CARTESIAN_POINT('Ctrl Pts',(-0.261929365828814,-1.9516045388674,
20.3316167966584));
#23143=CARTESIAN_POINT('Ctrl Pts',(-1.78167286399379,-0.838456368095613,
20.2204836786668));
#23144=CARTESIAN_POINT('Ctrl Pts',(-1.67075922179782,1.04208006884005,20.1093505606753));
#23145=CARTESIAN_POINT('Ctrl Pts',(-0.0307009971998217,1.96886381712767,
19.9982174426837));
#23146=CARTESIAN_POINT('Ctrl Pts',(1.6374560226953,1.09366589428439,19.8870843246922));
#23147=CARTESIAN_POINT('Ctrl Pts',(1.80694877506856,-0.782498078261772,
19.7759512067006));
#23148=CARTESIAN_POINT('Ctrl Pts',(0.322651014412248,-1.94248905501149,
19.664818088709));
#23149=CARTESIAN_POINT('Ctrl Pts',(-1.45694989770362,-1.32463750790632,
19.5536849707175));
#23150=CARTESIAN_POINT('Ctrl Pts',(-1.90309244999285,0.505574260069482,
19.4425518527259));
#23151=CARTESIAN_POINT('Ctrl Pts',(-0.607450787755709,1.87306488055063,
19.3314187347344));
#23152=CARTESIAN_POINT('Ctrl Pts',(1.24415547621381,1.52625219449683,19.2202856167428));
#23153=CARTESIAN_POINT('Ctrl Pts',(1.95705834927573,-0.217445409941707,
19.1091524987512));
#23154=CARTESIAN_POINT('Ctrl Pts',(0.878790793752254,-1.76213065216931,
18.9980193807597));
#23155=CARTESIAN_POINT('Ctrl Pts',(-1.00379299356237,-1.69404026652977,
18.8868862627681));
#23156=CARTESIAN_POINT('Ctrl Pts',(-1.96764225901355,-0.075505816270981,
18.7757531447766));
#23157=CARTESIAN_POINT('Ctrl Pts',(-1.13067338405636,1.61215041809436,18.664620026785));
#23158=CARTESIAN_POINT('Ctrl Pts',(0.741219758348873,1.8242725863998,18.5534869087934));
#23159=CARTESIAN_POINT('Ctrl Pts',(1.93455119820066,0.366807418669223,18.4423537908019));
#23160=CARTESIAN_POINT('Ctrl Pts',(1.3576286714496,-1.42648727235616,18.3312206728103));
#23161=CARTESIAN_POINT('Ctrl Pts',(-0.462471169546211,-1.91398750101902,
18.2200875548188));
#23162=CARTESIAN_POINT('Ctrl Pts',(-1.85810063661255,-0.650148800818648,
18.1089544368272));
#23163=CARTESIAN_POINT('Ctrl Pts',(-1.55545024827346,1.20953702335538,17.9978213188357));
#23164=CARTESIAN_POINT('Ctrl Pts',(0.175492742231552,1.96063858127948,17.8866882008441));
#23165=CARTESIAN_POINT('Ctrl Pts',(1.21513400202243,1.26723240811114,17.8125994555164));
#23166=CARTESIAN_POINT('Ctrl Pts',(1.47357822736256,0.777253631604911,17.7755550828525));
#23167=CARTESIAN_POINT('Ctrl Pts',(1.36778062465881,1.16331236980976,29.0748149723825));
#23168=CARTESIAN_POINT('Ctrl Pts',(1.75459305244158,0.708512302494195,29.0377705997186));
#23169=CARTESIAN_POINT('Ctrl Pts',(2.032169732279,-0.609441198611308,28.9636818543909));
#23170=CARTESIAN_POINT('Ctrl Pts',(0.587508218617532,-2.0407555346806,28.8525487363994));
#23171=CARTESIAN_POINT('Ctrl Pts',(-1.39455811083951,-1.59897576823537,
28.7414156184078));
#23172=CARTESIAN_POINT('Ctrl Pts',(-2.1003958292741,0.303598609901467,28.6302825004162));
#23173=CARTESIAN_POINT('Ctrl Pts',(-0.883806742378252,1.92967419483109,
28.5191493824247));
#23174=CARTESIAN_POINT('Ctrl Pts',(1.14164526753591,1.78892653264515,28.4080162644331));
#23175=CARTESIAN_POINT('Ctrl Pts',(2.12223508864335,0.0112517580134664,
28.2968831464416));
#23176=CARTESIAN_POINT('Ctrl Pts',(1.1604632516702,-1.77691290117273,28.18575002845));
#23177=CARTESIAN_POINT('Ctrl Pts',(-0.863405769384917,-1.93867716248943,
28.0746169104585));
#23178=CARTESIAN_POINT('Ctrl Pts',(-2.09705416621089,-0.326139671192082,
27.9634837924668));
#23179=CARTESIAN_POINT('Ctrl Pts',(-1.41139484462771,1.58492067337769,27.8523506744754));
#23180=CARTESIAN_POINT('Ctrl Pts',(0.566027963341392,2.04538519837037,27.7412175564837));
#23181=CARTESIAN_POINT('Ctrl Pts',(2.02540002692064,0.633839985216669,27.6300844384923));
#23182=CARTESIAN_POINT('Ctrl Pts',(1.63104609718075,-1.35782432740293,27.5189513205007));
#23183=CARTESIAN_POINT('Ctrl Pts',(-0.256105329778625,-2.10675239713451,
27.4078182025091));
#23184=CARTESIAN_POINT('Ctrl Pts',(-1.90885912462653,-0.92749877925752,
27.2966850845175));
#23185=CARTESIAN_POINT('Ctrl Pts',(-1.81454989277534,1.10063876165494,27.185551966526));
#23186=CARTESIAN_POINT('Ctrl Pts',(-0.059493191487418,2.121428109307,27.0744188485344));
#23187=CARTESIAN_POINT('Ctrl Pts',(1.75001402673825,1.20060309724918,26.9632857305429));
#23188=CARTESIAN_POINT('Ctrl Pts',(1.95783952445267,-0.8190611998569,26.8521526125513));
#23189=CARTESIAN_POINT('Ctrl Pts',(0.373773231322559,-2.08908840982359,
26.7410194945597));
#23190=CARTESIAN_POINT('Ctrl Pts',(-1.55238503559378,-1.44709970173515,
26.6298863765682));
#23191=CARTESIAN_POINT('Ctrl Pts',(-2.05773941618243,0.519331621246395,
26.5187532585766));
#23192=CARTESIAN_POINT('Ctrl Pts',(-0.679769691492573,2.01045019826922,
26.4076201405851));
#23193=CARTESIAN_POINT('Ctrl Pts',(1.32035201045348,1.66152562614826,26.2964870225936));
#23194=CARTESIAN_POINT('Ctrl Pts',(2.11203558381729,-0.208092597522944,
26.1853539046019));
#23195=CARTESIAN_POINT('Ctrl Pts',(0.970701061995584,-1.88725628472242,
26.0742207866104));
#23196=CARTESIAN_POINT('Ctrl Pts',(-1.05905727820396,-1.83912873886292,
25.9630876686188));
#23197=CARTESIAN_POINT('Ctrl Pts',(-2.11952471329362,-0.10775818358496,
25.8519545506273));
#23198=CARTESIAN_POINT('Ctrl Pts',(-1.24011970710203,1.72223690252185,25.7408214326357));
#23199=CARTESIAN_POINT('Ctrl Pts',(0.774291665667894,1.97597298891337,25.6296883146442));
#23200=CARTESIAN_POINT('Ctrl Pts',(2.08004083019426,0.421220822282945,25.5185551966526));
#23201=CARTESIAN_POINT('Ctrl Pts',(1.48205475731824,-1.51904921997551,25.407422078661));
#23202=CARTESIAN_POINT('Ctrl Pts',(-0.4723661625626,-2.06902562692568,25.2962889606695));
#23203=CARTESIAN_POINT('Ctrl Pts',(-1.99445897831498,-0.725348344054207,
25.1851558426779));
#23204=CARTESIAN_POINT('Ctrl Pts',(-1.69114443597316,1.28219629272614,25.0740227246863));
#23205=CARTESIAN_POINT('Ctrl Pts',(0.159972056967716,2.11622441565034,24.9628896066948));
#23206=CARTESIAN_POINT('Ctrl Pts',(1.86467582693291,1.01340065958943,24.8517564887032));
#23207=CARTESIAN_POINT('Ctrl Pts',(1.86275488716375,-1.0169272671887,24.7406233707117));
#23208=CARTESIAN_POINT('Ctrl Pts',(0.155967357344418,-2.11652333316869,
24.6294902527201));
#23209=CARTESIAN_POINT('Ctrl Pts',(-1.69356763673189,-1.27899393908601,
24.5183571347286));
#23210=CARTESIAN_POINT('Ctrl Pts',(-1.99308287149855,0.729121048759038,
24.407224016737));
#23211=CARTESIAN_POINT('Ctrl Pts',(-0.468450215292354,2.06991575485501,
24.2960908987455));
#23212=CARTESIAN_POINT('Ctrl Pts',(1.48492651597021,1.51624209101745,24.1849577807538));
#23213=CARTESIAN_POINT('Ctrl Pts',(2.0792400536787,-0.425156013226423,24.0738246627624));
#23214=CARTESIAN_POINT('Ctrl Pts',(0.770551256169416,-1.97743460018787,
23.9626915447708));
#23215=CARTESIAN_POINT('Ctrl Pts',(-1.24337637958803,-1.71988720998994,
23.8515584267792));
#23216=CARTESIAN_POINT('Ctrl Pts',(-2.11931701392909,0.111768648891705,
23.7404253087876));
#23217=CARTESIAN_POINT('Ctrl Pts',(-1.05557530161745,1.84112944113651,23.6292921907961));
#23218=CARTESIAN_POINT('Ctrl Pts',(0.9742704737735,1.88541610270454,23.5181590728045));
#23219=CARTESIAN_POINT('Ctrl Pts',(2.11242556465477,0.204095737822706,23.407025954813));
#23220=CARTESIAN_POINT('Ctrl Pts',(1.31720563450397,-1.66402107944443,23.2958928368214));
#23221=CARTESIAN_POINT('Ctrl Pts',(-0.68357273705343,-2.00916030957256,
23.1847597188299));
#23222=CARTESIAN_POINT('Ctrl Pts',(-2.05871843449878,-0.515436944600698,
23.0736266008383));
#23223=CARTESIAN_POINT('Ctrl Pts',(-1.54964399032288,1.45003459947016,22.9624934828467));
#23224=CARTESIAN_POINT('Ctrl Pts',(0.377725627189618,2.08837740530025,22.8513603648552));
#23225=CARTESIAN_POINT('Ctrl Pts',(1.95938588356236,0.81535501206587,22.7402272468636));
#23226=CARTESIAN_POINT('Ctrl Pts',(1.74773905862198,-1.20391238027174,22.6290941288721));
#23227=CARTESIAN_POINT('Ctrl Pts',(-0.0635073431082646,-2.12131177665513,
22.5179610108805));
#23228=CARTESIAN_POINT('Ctrl Pts',(-1.81662932480114,-1.09720314102583,
22.406827892889));
#23229=CARTESIAN_POINT('Ctrl Pts',(-1.90710064660258,0.931108994765127,
22.2956947748974));
#23230=CARTESIAN_POINT('Ctrl Pts',(-0.252118393883275,2.1072335304541,22.1845616569058));
#23231=CARTESIAN_POINT('Ctrl Pts',(1.63361253620114,1.35473499916799,22.0734285389142));
#23232=CARTESIAN_POINT('Ctrl Pts',(2.0241969747917,-0.63767032520673,21.9622954209227));
#23233=CARTESIAN_POINT('Ctrl Pts',(0.562156670435786,-2.04645466949263,
21.8511623029311));
#23234=CARTESIAN_POINT('Ctrl Pts',(-1.41439154497283,-1.58224315258837,
21.7400291849396));
#23235=CARTESIAN_POINT('Ctrl Pts',(-2.09643294851562,0.330099574049098,
21.628896066948));
#23236=CARTESIAN_POINT('Ctrl Pts',(-0.859736402776227,1.94032217792285,
21.5177629489565));
#23237=CARTESIAN_POINT('Ctrl Pts',(1.16382473767152,1.7746855542275,21.4066298309649));
#23238=CARTESIAN_POINT('Ctrl Pts',(2.12220767052146,-0.0152131396446604,
21.2954967129734));
#23239=CARTESIAN_POINT('Ctrl Pts',(1.13826261400238,-1.79118816932096,21.1843635949818));
#23240=CARTESIAN_POINT('Ctrl Pts',(-0.887465188378072,-1.92779728597407,
21.0732304769903));
#23241=CARTESIAN_POINT('Ctrl Pts',(-2.10094992016838,-0.300010449106,20.9620973589987));
#23242=CARTESIAN_POINT('Ctrl Pts',(-1.3915625922397,1.60235775901099,20.8509642410071));
#23243=CARTESIAN_POINT('Ctrl Pts',(0.591437591096275,2.03818507802715,20.7398311230155));
#23244=CARTESIAN_POINT('Ctrl Pts',(2.03313081303557,0.608585191194508,20.628698005024));
#23245=CARTESIAN_POINT('Ctrl Pts',(1.6140226902295,-1.378015815808,20.5175648870324));
#23246=CARTESIAN_POINT('Ctrl Pts',(-0.282302523284989,-2.10340251095318,
20.4064317690409));
#23247=CARTESIAN_POINT('Ctrl Pts',(-1.92025336136826,-0.903672437142665,
20.2952986510493));
#23248=CARTESIAN_POINT('Ctrl Pts',(-1.80071273269696,1.12313421585117,20.1841655330578));
#23249=CARTESIAN_POINT('Ctrl Pts',(-0.0330889549151928,2.12200423507653,
20.0730324150662));
#23250=CARTESIAN_POINT('Ctrl Pts',(1.76481917372027,1.17873244418496,19.9618992970747));
#23251=CARTESIAN_POINT('Ctrl Pts',(1.94749526092448,-0.843361649275031,
19.8507661790831));
#23252=CARTESIAN_POINT('Ctrl Pts',(0.347747169244733,-2.09357801462248,
19.7396330610915));
#23253=CARTESIAN_POINT('Ctrl Pts',(-1.5702730815236,-1.42766928685762,19.6284999431));
#23254=CARTESIAN_POINT('Ctrl Pts',(-2.05111709783893,0.544898388441233,
19.5173668251084));
#23255=CARTESIAN_POINT('Ctrl Pts',(-0.654698985782925,2.01875395064148,
19.4062337071168));
#23256=CARTESIAN_POINT('Ctrl Pts',(1.34092727320823,1.64496578805638,19.2951005891253));
#23257=CARTESIAN_POINT('Ctrl Pts',(2.10928052480214,-0.234358555823027,
19.1839674711337));
#23258=CARTESIAN_POINT('Ctrl Pts',(0.947144119296707,-1.89919113456843,
19.0728343531422));
#23259=CARTESIAN_POINT('Ctrl Pts',(-1.08186912926612,-1.82580460298704,
18.9617012351506));
#23260=CARTESIAN_POINT('Ctrl Pts',(-2.12068766281338,-0.0813787426566056,
18.8505681171591));
#23261=CARTESIAN_POINT('Ctrl Pts',(-1.21861841768019,1.73754527104238,18.7394349991675));
#23262=CARTESIAN_POINT('Ctrl Pts',(0.798872655719443,1.96616653757285,18.6283018811759));
#23263=CARTESIAN_POINT('Ctrl Pts',(2.08502274247847,0.395338107746388,18.5171687631844));
#23264=CARTESIAN_POINT('Ctrl Pts',(1.46322653980215,-1.53744103928863,18.4060356451928));
#23265=CARTESIAN_POINT('Ctrl Pts',(-0.498442691587246,-2.06285957805406,
18.2949025272013));
#23266=CARTESIAN_POINT('Ctrl Pts',(-2.00262577116299,-0.700718097801093,
18.1837694092097));
#23267=CARTESIAN_POINT('Ctrl Pts',(-1.67643489893699,1.30361615857535,18.0726362912181));
#23268=CARTESIAN_POINT('Ctrl Pts',(0.189142762948342,2.11313923123394,17.9615031732266));
#23269=CARTESIAN_POINT('Ctrl Pts',(1.30964847646945,1.36579915454035,17.8874144278989));
#23270=CARTESIAN_POINT('Ctrl Pts',(1.58819478116152,0.83770928372304,17.850370055235));
#23271=CARTESIAN_POINT('Ctrl Pts',(1.46649036946526,1.24726608657098,29.149629944765));
#23272=CARTESIAN_POINT('Ctrl Pts',(1.88121820659513,0.759644090231628,29.1125855721011));
#23273=CARTESIAN_POINT('Ctrl Pts',(2.1788269900733,-0.653423240837164,29.0384968267735));
#23274=CARTESIAN_POINT('Ctrl Pts',(0.629907405508992,-2.18803241111019,
28.9273637087818));
#23275=CARTESIAN_POINT('Ctrl Pts',(-1.49520032842689,-1.71437036236012,
28.8162305907904));
#23276=CARTESIAN_POINT('Ctrl Pts',(-2.25197681570011,0.325508659485947,
28.7050974727987));
#23277=CARTESIAN_POINT('Ctrl Pts',(-0.947589147557543,2.06893457321149,
28.5939643548072));
#23278=CARTESIAN_POINT('Ctrl Pts',(1.22403531677795,1.91802945919006,28.4828312368156));
#23279=CARTESIAN_POINT('Ctrl Pts',(2.27539216679067,0.0120637728513067,
28.3716981188241));
#23280=CARTESIAN_POINT('Ctrl Pts',(1.2442113537887,-1.90514883013378,28.2605650008325));
#23281=CARTESIAN_POINT('Ctrl Pts',(-0.925715880834006,-2.07858726541193,
28.1494318828409));
#23282=CARTESIAN_POINT('Ctrl Pts',(-2.24839399210117,-0.349676460012044,
28.0382987648494));
#23283=CARTESIAN_POINT('Ctrl Pts',(-1.51325213257481,1.69930094195811,27.9271656468578));
#23284=CARTESIAN_POINT('Ctrl Pts',(0.606876967054013,2.19299618753202,27.8160325288663));
#23285=CARTESIAN_POINT('Ctrl Pts',(2.1715687298427,0.67958283466262,27.7048994108747));
#23286=CARTESIAN_POINT('Ctrl Pts',(1.74875513700607,-1.45581554794925,27.5937662928831));
#23287=CARTESIAN_POINT('Ctrl Pts',(-0.274587892910651,-2.25879212320052,
27.4826331748916));
#23288=CARTESIAN_POINT('Ctrl Pts',(-2.04661732478405,-0.994434343454176,
27.3715000569));
#23289=CARTESIAN_POINT('Ctrl Pts',(-1.94550200134107,1.18006946079512,27.2603669389085));
#23290=CARTESIAN_POINT('Ctrl Pts',(-0.0637866853734778,2.27452694951549,
27.1492338209169));
#23291=CARTESIAN_POINT('Ctrl Pts',(1.8763087225928,1.28724800448557,27.0381007029253));
#23292=CARTESIAN_POINT('Ctrl Pts',(2.09913253324851,-0.878171060430411,
26.9269675849338));
#23293=CARTESIAN_POINT('Ctrl Pts',(0.400747630297199,-2.23985336444724,
26.8158344669422));
#23294=CARTESIAN_POINT('Ctrl Pts',(-1.66441727814951,-1.55153373135404,
26.7047013489507));
#23295=CARTESIAN_POINT('Ctrl Pts',(-2.20624198230131,0.556810651786059,
26.5935682309591));
#23296=CARTESIAN_POINT('Ctrl Pts',(-0.728827187676307,2.1555400046603,26.4824351129675));
#23297=CARTESIAN_POINT('Ctrl Pts',(1.41563893560571,1.78143430710897,26.371301994976));
#23298=CARTESIAN_POINT('Ctrl Pts',(2.26445658594454,-0.223110186474918,
26.2601688769844));
#23299=CARTESIAN_POINT('Ctrl Pts',(1.04075444072131,-2.02345545503584,26.1490357589928));
#23300=CARTESIAN_POINT('Ctrl Pts',(-1.13548713236497,-1.97185464914889,
26.0379026410014));
#23301=CARTESIAN_POINT('Ctrl Pts',(-2.27248618956277,-0.115534856693729,
25.9267695230097));
#23302=CARTESIAN_POINT('Ctrl Pts',(-1.32961644189312,1.84652698389845,25.8156364050182));
#23303=CARTESIAN_POINT('Ctrl Pts',(0.830170606593015,2.11857465029362,25.7045032870266));
#23304=CARTESIAN_POINT('Ctrl Pts',(2.23015284072714,0.451619410422826,25.5933701690351));
#23305=CARTESIAN_POINT('Ctrl Pts',(1.58901141706808,-1.62867568941729,25.4822370510435));
#23306=CARTESIAN_POINT('Ctrl Pts',(-0.506455798371986,-2.21834269426078,
25.371103933052));
#23307=CARTESIAN_POINT('Ctrl Pts',(-2.13839473323584,-0.777695152194749,
25.2599708150604));
#23308=CARTESIAN_POINT('Ctrl Pts',(-1.81319064184582,1.37472960294051,25.1488376970688));
#23309=CARTESIAN_POINT('Ctrl Pts',(0.17151689144977,2.26894771663592,25.0377045790773));
#23310=CARTESIAN_POINT('Ctrl Pts',(1.99924541485144,1.08653557515362,24.9265714610857));
#23311=CARTESIAN_POINT('Ctrl Pts',(1.99718584504836,-1.09031669033245,24.8154383430942));
#23312=CARTESIAN_POINT('Ctrl Pts',(0.167223181388163,-2.26926820637968,
24.7043052251026));
#23313=CARTESIAN_POINT('Ctrl Pts',(-1.81578871971876,-1.37129614242191,
24.5931721071111));
#23314=CARTESIAN_POINT('Ctrl Pts',(-2.13691931579151,0.781740124770563,
24.4820389891195));
#23315=CARTESIAN_POINT('Ctrl Pts',(-0.502257245727199,2.21929706078156,
24.370905871128));
#23316=CARTESIAN_POINT('Ctrl Pts',(1.59209042427919,1.62566597608415,24.2597727531364));
#23317=CARTESIAN_POINT('Ctrl Pts',(2.22929427391681,-0.455838595514776,
24.1486396351449));
#23318=CARTESIAN_POINT('Ctrl Pts',(0.826160259898167,-2.1201417428663,24.0375065171532));
#23319=CARTESIAN_POINT('Ctrl Pts',(-1.33310814133023,-1.84400771918075,
23.9263733991618));
#23320=CARTESIAN_POINT('Ctrl Pts',(-2.27226350098807,0.119834748535584,
23.8152402811701));
#23321=CARTESIAN_POINT('Ctrl Pts',(-1.13175386912174,1.97399973774241,23.7041071631786));
#23322=CARTESIAN_POINT('Ctrl Pts',(1.04458144916301,2.02148247109483,23.592974045187));
#23323=CARTESIAN_POINT('Ctrl Pts',(2.26487471084858,0.218824882126523,23.4818409271955));
#23324=CARTESIAN_POINT('Ctrl Pts',(1.41226549256559,-1.78410985182741,23.3707078092039));
#23325=CARTESIAN_POINT('Ctrl Pts',(-0.732904690741557,-2.15415702750941,
23.2595746912124));
#23326=CARTESIAN_POINT('Ctrl Pts',(-2.2072916542345,-0.552634904820408,
23.1484415732208));
#23327=CARTESIAN_POINT('Ctrl Pts',(-1.66147841761912,1.55468043425812,23.0373084552292));
#23328=CARTESIAN_POINT('Ctrl Pts',(0.404985261954545,2.23909104827802,22.9261753372377));
#23329=CARTESIAN_POINT('Ctrl Pts',(2.10079048972282,0.874197405149011,22.8150422192461));
#23330=CARTESIAN_POINT('Ctrl Pts',(1.87386957498886,-1.29079611124694,22.7039091012546));
#23331=CARTESIAN_POINT('Ctrl Pts',(-0.0680905295626852,-2.27440222138984,
22.592775983263));
#23332=CARTESIAN_POINT('Ctrl Pts',(-1.9477315014413,-1.17638589891765,22.4816428652714));
#23333=CARTESIAN_POINT('Ctrl Pts',(-2.04473194123603,0.998305100341762,
22.3705097472799));
#23334=CARTESIAN_POINT('Ctrl Pts',(-0.270313228546498,2.25930797886252,
22.2593766292883));
#23335=CARTESIAN_POINT('Ctrl Pts',(1.75150679033363,1.45250326963284,22.1482435112967));
#23336=CARTESIAN_POINT('Ctrl Pts',(2.17027885606524,-0.683689601936504,
22.0371103933052));
#23337=CARTESIAN_POINT('Ctrl Pts',(0.60272629138198,-2.19414284005285,21.9259772753136));
#23338=CARTESIAN_POINT('Ctrl Pts',(-1.51646509824859,-1.6964301903326,21.8148441573221));
#23339=CARTESIAN_POINT('Ctrl Pts',(-2.2477279424796,0.353922140422439,21.7037110393305));
#23340=CARTESIAN_POINT('Ctrl Pts',(-0.921781704039374,2.0803509980217,21.592577921339));
#23341=CARTESIAN_POINT('Ctrl Pts',(1.24781543090395,1.90276074041694,21.4814448033474));
#23342=CARTESIAN_POINT('Ctrl Pts',(2.27536276996272,-0.0163110387557863,
21.3703116853558));
#23343=CARTESIAN_POINT('Ctrl Pts',(1.22040854451584,-1.92045431325255,21.2591785673643));
#23344=CARTESIAN_POINT('Ctrl Pts',(-0.951511615626781,-2.06692221193544,
21.1480454493727));
#23345=CARTESIAN_POINT('Ctrl Pts',(-2.25257089412586,-0.321661548950983,
21.0369123313812));
#23346=CARTESIAN_POINT('Ctrl Pts',(-1.49198862978241,1.71799642403453,20.9257792133896));
#23347=CARTESIAN_POINT('Ctrl Pts',(0.634120352230293,2.18527645020575,20.814646095398));
#23348=CARTESIAN_POINT('Ctrl Pts',(2.17985742993213,0.652505457231891,20.7035129774065));
#23349=CARTESIAN_POINT('Ctrl Pts',(1.73050318790003,-1.47746421203863,20.5923798594149));
#23350=CARTESIAN_POINT('Ctrl Pts',(-0.302675680741162,-2.25520048303895,
20.4812467414234));
#23351=CARTESIAN_POINT('Ctrl Pts',(-2.05883385874272,-0.968888506189718,
20.3701136234318));
#23352=CARTESIAN_POINT('Ctrl Pts',(-1.9306662435961,1.20418836286229,20.2589805054403));
#23353=CARTESIAN_POINT('Ctrl Pts',(-0.0354769126305643,2.27514465302538,
20.1478473874487));
#23354=CARTESIAN_POINT('Ctrl Pts',(1.89218232474523,1.26379899408554,20.0367142694571));
#23355=CARTESIAN_POINT('Ctrl Pts',(2.0880417467804,-0.904225220288291,19.9255811514656));
#23356=CARTESIAN_POINT('Ctrl Pts',(0.372843324077218,-2.24466697423347,
19.814448033474));
#23357=CARTESIAN_POINT('Ctrl Pts',(-1.68359626534358,-1.53070106580892,
19.7033149154824));
#23358=CARTESIAN_POINT('Ctrl Pts',(-2.19914174568501,0.584222516812984,
19.5921817974909));
#23359=CARTESIAN_POINT('Ctrl Pts',(-0.701947183810143,2.16444302073233,
19.4810486794993));
#23360=CARTESIAN_POINT('Ctrl Pts',(1.43769907020265,1.76367938161593,19.3699155615078));
#23361=CARTESIAN_POINT('Ctrl Pts',(2.26150270032853,-0.251271701704347,
19.2587824435162));
#23362=CARTESIAN_POINT('Ctrl Pts',(1.01549744484116,-2.03625161696756,19.1476493255247));
#23363=CARTESIAN_POINT('Ctrl Pts',(-1.15994526496988,-1.95756893944432,
19.0365162075331));
#23364=CARTESIAN_POINT('Ctrl Pts',(-2.2737330666132,-0.087251669042228,
18.9253830895416));
#23365=CARTESIAN_POINT('Ctrl Pts',(-1.30656345130402,1.86294012399039,18.81424997155));
#23366=CARTESIAN_POINT('Ctrl Pts',(0.856525553090016,2.1080604887459,18.7031168535584));
#23367=CARTESIAN_POINT('Ctrl Pts',(2.23549428675628,0.423868796823551,18.5919837355669));
#23368=CARTESIAN_POINT('Ctrl Pts',(1.5688244081547,-1.6483948062211,18.4808506175753));
#23369=CARTESIAN_POINT('Ctrl Pts',(-0.53441421362828,-2.2117316550891,18.3697174995838));
#23370=CARTESIAN_POINT('Ctrl Pts',(-2.14715090571344,-0.751287394783537,
18.2585843815922));
#23371=CARTESIAN_POINT('Ctrl Pts',(-1.79741954960052,1.39769529379532,18.1474512636006));
#23372=CARTESIAN_POINT('Ctrl Pts',(0.202792783665131,2.2656398811884,18.0363181456091));
#23373=CARTESIAN_POINT('Ctrl Pts',(1.40416295091648,1.46436590096956,17.9622294002814));
#23374=CARTESIAN_POINT('Ctrl Pts',(1.70281133496047,0.898164935841169,17.9251850276175));
#23375=CARTESIAN_POINT('Ctrl Pts',(1.5652001142717,1.33121980333221,29.2244449171475));
#23376=CARTESIAN_POINT('Ctrl Pts',(2.00784336074869,0.810775877969061,29.1874005444836));
#23377=CARTESIAN_POINT('Ctrl Pts',(2.32548424786761,-0.697405283063022,
29.1133117991559));
#23378=CARTESIAN_POINT('Ctrl Pts',(0.67230659240045,-2.33530928753977,29.0021786811644));
#23379=CARTESIAN_POINT('Ctrl Pts',(-1.59584254601428,-1.82976495648487,
28.8910455631728));
#23380=CARTESIAN_POINT('Ctrl Pts',(-2.40355780212611,0.347418709070426,
28.7799124451812));
#23381=CARTESIAN_POINT('Ctrl Pts',(-1.01137155273683,2.20819495159188,28.6687793271897));
#23382=CARTESIAN_POINT('Ctrl Pts',(1.30642536602,2.04713238573498,28.5576462091981));
#23383=CARTESIAN_POINT('Ctrl Pts',(2.428549244938,0.0128757876891458,28.4465130912066));
#23384=CARTESIAN_POINT('Ctrl Pts',(1.32795945590719,-2.03338475909482,28.335379973215));
#23385=CARTESIAN_POINT('Ctrl Pts',(-0.988025992283097,-2.21849736833443,
28.2242468552234));
#23386=CARTESIAN_POINT('Ctrl Pts',(-2.39973381799145,-0.373213248832005,
28.1131137372319));
#23387=CARTESIAN_POINT('Ctrl Pts',(-1.61510942052191,1.81368121053853,28.0019806192403));
#23388=CARTESIAN_POINT('Ctrl Pts',(0.647725970766636,2.34060717669366,27.8908475012488));
#23389=CARTESIAN_POINT('Ctrl Pts',(2.31773743276476,0.725325684108574,27.7797143832572));
#23390=CARTESIAN_POINT('Ctrl Pts',(1.86646417683138,-1.55380676849557,27.6685812652656));
#23391=CARTESIAN_POINT('Ctrl Pts',(-0.293070456042677,-2.41083184926652,
27.5574481472741));
#23392=CARTESIAN_POINT('Ctrl Pts',(-2.18437552494158,-1.06136990765084,
27.4463150292825));
#23393=CARTESIAN_POINT('Ctrl Pts',(-2.07645410990679,1.2595001599353,27.335181911291));
#23394=CARTESIAN_POINT('Ctrl Pts',(-0.0680801792595378,2.42762578972398,
27.2240487932994));
#23395=CARTESIAN_POINT('Ctrl Pts',(2.00260341844735,1.37389291172196,27.1129156753079));
#23396=CARTESIAN_POINT('Ctrl Pts',(2.24042554204435,-0.937280921003925,
27.0017825573163));
#23397=CARTESIAN_POINT('Ctrl Pts',(0.427722029271838,-2.39061831907088,
26.8906494393248));
#23398=CARTESIAN_POINT('Ctrl Pts',(-1.77644952070524,-1.65596776097293,
26.7795163213331));
#23399=CARTESIAN_POINT('Ctrl Pts',(-2.3547445484202,0.594289682325723,26.6683832033416));
#23400=CARTESIAN_POINT('Ctrl Pts',(-0.777884683860044,2.30062981105139,
26.5572500853501));
#23401=CARTESIAN_POINT('Ctrl Pts',(1.51092586075795,1.90134298806969,26.4461169673585));
#23402=CARTESIAN_POINT('Ctrl Pts',(2.4168775880718,-0.238127775426892,26.3349838493669));
#23403=CARTESIAN_POINT('Ctrl Pts',(1.11080781944703,-2.15965462534927,26.2238507313753));
#23404=CARTESIAN_POINT('Ctrl Pts',(-1.21191698652597,-2.10458055943487,
26.1127176133838));
#23405=CARTESIAN_POINT('Ctrl Pts',(-2.42544766583193,-0.123311529802495,
26.0015844953922));
#23406=CARTESIAN_POINT('Ctrl Pts',(-1.41911317668421,1.97081706527504,25.8904513774007));
#23407=CARTESIAN_POINT('Ctrl Pts',(0.886049547518136,2.26117631167387,25.7793182594091));
#23408=CARTESIAN_POINT('Ctrl Pts',(2.38026485126002,0.482017998562706,25.6681851414176));
#23409=CARTESIAN_POINT('Ctrl Pts',(1.69596807681793,-1.73830215885906,25.557052023426));
#23410=CARTESIAN_POINT('Ctrl Pts',(-0.540545434181373,-2.36765976159588,
25.4459189054345));
#23411=CARTESIAN_POINT('Ctrl Pts',(-2.2823304881567,-0.830041960335293,
25.3347857874429));
#23412=CARTESIAN_POINT('Ctrl Pts',(-1.93523684771849,1.46726291315489,25.2236526694514));
#23413=CARTESIAN_POINT('Ctrl Pts',(0.183061725931824,2.4216710176215,25.1125195514598));
#23414=CARTESIAN_POINT('Ctrl Pts',(2.13381500276998,1.15967049071781,25.0013864334682));
#23415=CARTESIAN_POINT('Ctrl Pts',(2.13161680293297,-1.1637061134762,24.8902533154767));
#23416=CARTESIAN_POINT('Ctrl Pts',(0.178479005431905,-2.42201307959068,
24.7791201974851));
#23417=CARTESIAN_POINT('Ctrl Pts',(-1.93800980270562,-1.46359834575782,
24.6679870794936));
#23418=CARTESIAN_POINT('Ctrl Pts',(-2.28075576008446,0.834359200782086,
24.556853961502));
#23419=CARTESIAN_POINT('Ctrl Pts',(-0.536064276162042,2.36867836670812,
24.4457208435105));
#23420=CARTESIAN_POINT('Ctrl Pts',(1.69925433258817,1.73508986115085,24.3345877255189));
#23421=CARTESIAN_POINT('Ctrl Pts',(2.37934849415491,-0.486521177803125,
24.2234546075274));
#23422=CARTESIAN_POINT('Ctrl Pts',(0.881769263626921,-2.26284888554473,
24.1123214895357));
#23423=CARTESIAN_POINT('Ctrl Pts',(-1.42283990307244,-1.96812822837156,
24.0011883715443));
#23424=CARTESIAN_POINT('Ctrl Pts',(-2.42520998804704,0.127900848179458,
23.8900552535526));
#23425=CARTESIAN_POINT('Ctrl Pts',(-1.20793243662604,2.10687003434831,23.7789221355611));
#23426=CARTESIAN_POINT('Ctrl Pts',(1.11489242455252,2.15754883948512,23.6677890175695));
#23427=CARTESIAN_POINT('Ctrl Pts',(2.4173238570424,0.233554026430338,23.556655899578));
#23428=CARTESIAN_POINT('Ctrl Pts',(1.50732535062721,-1.90419862421039,23.4455227815864));
#23429=CARTESIAN_POINT('Ctrl Pts',(-0.782236644429685,-2.29915374544626,
23.3343896635949));
#23430=CARTESIAN_POINT('Ctrl Pts',(-2.35586487397022,-0.589832865040116,
23.2232565456033));
#23431=CARTESIAN_POINT('Ctrl Pts',(-1.77331284491536,1.65932626904607,23.1121234276117));
#23432=CARTESIAN_POINT('Ctrl Pts',(0.43224489671947,2.38980469125578,23.0009903096202));
#23433=CARTESIAN_POINT('Ctrl Pts',(2.24219509588329,0.933039798232153,22.8898571916286));
#23434=CARTESIAN_POINT('Ctrl Pts',(2.00000009135574,-1.37767984222214,22.778724073637));
#23435=CARTESIAN_POINT('Ctrl Pts',(-0.072673716017103,-2.42749266612454,
22.6675909556455));
#23436=CARTESIAN_POINT('Ctrl Pts',(-2.07883367808147,-1.25556865680948,
22.5564578376539));
#23437=CARTESIAN_POINT('Ctrl Pts',(-2.18236323586949,1.0655012059184,22.4453247196624));
#23438=CARTESIAN_POINT('Ctrl Pts',(-0.288508063209722,2.41138242727093,
22.3341916016708));
#23439=CARTESIAN_POINT('Ctrl Pts',(1.86940104446612,1.5502715400977,22.2230584836792));
#23440=CARTESIAN_POINT('Ctrl Pts',(2.31636073733878,-0.729708878666279,
22.1119253656877));
#23441=CARTESIAN_POINT('Ctrl Pts',(0.643295912328174,-2.34183101061307,
22.0007922476961));
#23442=CARTESIAN_POINT('Ctrl Pts',(-1.61853865152434,-1.81061722807683,
21.8896591297046));
#23443=CARTESIAN_POINT('Ctrl Pts',(-2.39902293644358,0.377744706795778,
21.778526011713));
#23444=CARTESIAN_POINT('Ctrl Pts',(-0.983827005302519,2.22037981812055,
21.6673928937214));
#23445=CARTESIAN_POINT('Ctrl Pts',(1.33180612413638,2.03083592660637,21.5562597757299));
#23446=CARTESIAN_POINT('Ctrl Pts',(2.42851786940399,-0.0174089378669135,
21.4451266577383));
#23447=CARTESIAN_POINT('Ctrl Pts',(1.30255447502931,-2.04972045718415,21.3339935397468));
#23448=CARTESIAN_POINT('Ctrl Pts',(-1.01555804287549,-2.20604713789681,
21.2228604217552));
#23449=CARTESIAN_POINT('Ctrl Pts',(-2.40419186808334,-0.343312648795965,
21.1117273037636));
#23450=CARTESIAN_POINT('Ctrl Pts',(-1.59241466732511,1.83363508905806,21.0005941857721));
#23451=CARTESIAN_POINT('Ctrl Pts',(0.676803113364313,2.33236782238435,20.8894610677805));
#23452=CARTESIAN_POINT('Ctrl Pts',(2.3265840468287,0.696425723269271,20.778327949789));
#23453=CARTESIAN_POINT('Ctrl Pts',(1.84698368557056,-1.57691260826926,20.6671948317974));
#23454=CARTESIAN_POINT('Ctrl Pts',(-0.323048838197336,-2.40699845512473,
20.5560617138059));
#23455=CARTESIAN_POINT('Ctrl Pts',(-2.19741435611719,-1.03410457523677,
20.4449285958143));
#23456=CARTESIAN_POINT('Ctrl Pts',(-2.06061975449524,1.2852425098734,20.3337954778227));
#23457=CARTESIAN_POINT('Ctrl Pts',(-0.037864870345937,2.42828507097424,
20.2226623598312));
#23458=CARTESIAN_POINT('Ctrl Pts',(2.01954547577021,1.34886554398611,20.1115292418396));
#23459=CARTESIAN_POINT('Ctrl Pts',(2.22858823263633,-0.965088791301547,
20.0003961238481));
#23460=CARTESIAN_POINT('Ctrl Pts',(0.397939478909703,-2.39575593384446,
19.8892630058565));
#23461=CARTESIAN_POINT('Ctrl Pts',(-1.79691944916357,-1.63373284476021,
19.7781298878649));
#23462=CARTESIAN_POINT('Ctrl Pts',(-2.34716639353109,0.623546645184736,
19.6669967698734));
#23463=CARTESIAN_POINT('Ctrl Pts',(-0.74919538183736,2.31013209082318,19.5558636518818));
#23464=CARTESIAN_POINT('Ctrl Pts',(1.53447086719707,1.88239297517548,19.4447305338903));
#23465=CARTESIAN_POINT('Ctrl Pts',(2.41372487585493,-0.268184847585669,
19.3335974158987));
#23466=CARTESIAN_POINT('Ctrl Pts',(1.08385077038562,-2.17331209936668,19.2224642979071));
#23467=CARTESIAN_POINT('Ctrl Pts',(-1.23802140067364,-2.08933327590159,
19.1113311799156));
#23468=CARTESIAN_POINT('Ctrl Pts',(-2.42677847041303,-0.0931245954278493,
19.000198061924));
#23469=CARTESIAN_POINT('Ctrl Pts',(-1.39450848492785,1.98833497693841,18.8890649439325));
#23470=CARTESIAN_POINT('Ctrl Pts',(0.91417845046059,2.24995443991895,18.7779318259409));
#23471=CARTESIAN_POINT('Ctrl Pts',(2.38596583103409,0.452399485900713,18.6667987079494));
#23472=CARTESIAN_POINT('Ctrl Pts',(1.67442227650725,-1.75934857315356,18.5556655899578));
#23473=CARTESIAN_POINT('Ctrl Pts',(-0.570385735669315,-2.36060373212415,
18.4445324719663));
#23474=CARTESIAN_POINT('Ctrl Pts',(-2.29167604026388,-0.801856691765977,
18.3333993539747));
#23475=CARTESIAN_POINT('Ctrl Pts',(-1.91840420026404,1.49177442901529,18.2222662359831));
#23476=CARTESIAN_POINT('Ctrl Pts',(0.216442804381921,2.41814053114287,18.1111331179916));
#23477=CARTESIAN_POINT('Ctrl Pts',(1.4986774253635,1.56293264739877,18.0370443726639));
#23478=CARTESIAN_POINT('Ctrl Pts',(1.81742788875943,0.958620587959298,18.));
#23479=CARTESIAN_POINT('Ctrl Pts',(1.26907087985237,1.07935865304853,29.));
#23480=CARTESIAN_POINT('Ctrl Pts',(1.3144094872273,1.03706254429827,29.));
#23481=CARTESIAN_POINT('Ctrl Pts',(1.35701863562271,0.992198004702034,29.));
#23482=CARTESIAN_POINT('Ctrl Pts',(1.39689941920223,0.945109875853942,29.));
#23483=CARTESIAN_POINT('Ctrl Pts',(1.43940262027365,0.894925400302773,29.));
#23484=CARTESIAN_POINT('Ctrl Pts',(1.47880756852856,0.842215055268869,29.));
#23485=CARTESIAN_POINT('Ctrl Pts',(1.51508678956216,0.787341601735945,29.));
#23486=CARTESIAN_POINT('Ctrl Pts',(1.54683110796656,0.739327329894636,29.));
#23487=CARTESIAN_POINT('Ctrl Pts',(1.57618204898653,0.689655703631122,29.));
#23488=CARTESIAN_POINT('Ctrl Pts',(1.60309832979504,0.638542209490663,29.));
#23489=CARTESIAN_POINT('Ctrl Pts',(1.61660467751284,0.612893917668903,29.));
#23490=CARTESIAN_POINT('Ctrl Pts',(1.62949763128333,0.586882216194757,29.));
#23491=CARTESIAN_POINT('Ctrl Pts',(1.64176963246512,0.560532489670278,29.));
#23492=CARTESIAN_POINT('Ctrl Pts',(1.64737448368887,0.548498079408378,29.));
#23493=CARTESIAN_POINT('Ctrl Pts',(1.65285037736292,0.536391499107776,29.));
#23494=CARTESIAN_POINT('Ctrl Pts',(1.65818810198435,0.524235070687702,29.));
#23495=CARTESIAN_POINT('Ctrl Pts',(1.68511823217932,0.462902907026757,29.));
#23496=CARTESIAN_POINT('Ctrl Pts',(1.70858664543798,0.400195370245674,29.));
#23497=CARTESIAN_POINT('Ctrl Pts',(1.72856940504418,0.336469942157596,29.));
#23498=CARTESIAN_POINT('Ctrl Pts',(1.7489050278493,0.271619226128731,29.));
#23499=CARTESIAN_POINT('Ctrl Pts',(1.76563136617229,0.205713511440919,29.));
#23500=CARTESIAN_POINT('Ctrl Pts',(1.77868388077386,0.139093051206905,29.));
#23501=CARTESIAN_POINT('Ctrl Pts',(1.7895994088527,0.0833798398826602,29.));
#23502=CARTESIAN_POINT('Ctrl Pts',(1.79794505461674,0.0271658230940875,
29.));
#23503=CARTESIAN_POINT('Ctrl Pts',(1.80365825317042,-0.0293622786831205,
29.));
#23504=CARTESIAN_POINT('Ctrl Pts',(1.80629075136643,-0.0554090061956506,
29.));
#23505=CARTESIAN_POINT('Ctrl Pts',(1.80836401037494,-0.0815225313140194,
29.));
#23506=CARTESIAN_POINT('Ctrl Pts',(1.8098701058109,-0.107684989121531,29.));
#23507=CARTESIAN_POINT('Ctrl Pts',(1.81052758192083,-0.119106038926533,
29.));
#23508=CARTESIAN_POINT('Ctrl Pts',(1.81107685493986,-0.130536175706242,
29.));
#23509=CARTESIAN_POINT('Ctrl Pts',(1.81151693302746,-0.141959838006402,
29.));
#23510=CARTESIAN_POINT('Ctrl Pts',(1.81421811506976,-0.212077829181081,
29.));
#23511=CARTESIAN_POINT('Ctrl Pts',(1.81281756748119,-0.282083201198475,
29.));
#23512=CARTESIAN_POINT('Ctrl Pts',(1.80726021940794,-0.351615623243351,
29.));
#23513=CARTESIAN_POINT('Ctrl Pts',(1.80229344163224,-0.413758948432297,
29.));
#23514=CARTESIAN_POINT('Ctrl Pts',(1.79400604326908,-0.475525464431958,
29.));
#23515=CARTESIAN_POINT('Ctrl Pts',(1.78232561606514,-0.536670064275249,
29.));
#23516=CARTESIAN_POINT('Ctrl Pts',(1.76959660145245,-0.603303800465088,
29.));
#23517=CARTESIAN_POINT('Ctrl Pts',(1.75283909722983,-0.669199777224924,
29.));
#23518=CARTESIAN_POINT('Ctrl Pts',(1.73229861749773,-0.734144131843436,
29.));
#23519=CARTESIAN_POINT('Ctrl Pts',(1.72436741483446,-0.759220802156505,
29.));
#23520=CARTESIAN_POINT('Ctrl Pts',(1.71587164297147,-0.784155545451161,
29.));
#23521=CARTESIAN_POINT('Ctrl Pts',(1.70682342442655,-0.808935730194906,
29.));
#23522=CARTESIAN_POINT('Ctrl Pts',(1.70285503775051,-0.819803875618098,
29.));
#23523=CARTESIAN_POINT('Ctrl Pts',(1.6987804849517,-0.830641729526751,29.));
#23524=CARTESIAN_POINT('Ctrl Pts',(1.69460587821655,-0.841435680151886,
29.));
#23525=CARTESIAN_POINT('Ctrl Pts',(1.6693812505011,-0.906657005984914,29.));
#23526=CARTESIAN_POINT('Ctrl Pts',(1.64046524049148,-0.970394630379315,
29.));
#23527=CARTESIAN_POINT('Ctrl Pts',(1.60817079267237,-1.03242943870664,29.));
#23528=CARTESIAN_POINT('Ctrl Pts',(1.57512648034544,-1.09590467113643,29.));
#23529=CARTESIAN_POINT('Ctrl Pts',(1.53854471445853,-1.15759791168999,29.));
#23530=CARTESIAN_POINT('Ctrl Pts',(1.49870459830356,-1.21727074006036,29.));
#23531=CARTESIAN_POINT('Ctrl Pts',(1.46819625766185,-1.26296636423716,29.));
#23532=CARTESIAN_POINT('Ctrl Pts',(1.43577599564766,-1.30747724665079,29.));
#23533=CARTESIAN_POINT('Ctrl Pts',(1.40154956798818,-1.35069022138389,29.));
#23534=CARTESIAN_POINT('Ctrl Pts',(1.38024570649905,-1.37758765974371,29.));
#23535=CARTESIAN_POINT('Ctrl Pts',(1.35824175768608,-1.40398212651681,29.));
#23536=CARTESIAN_POINT('Ctrl Pts',(1.33556031487129,-1.42984464135766,29.));
#23537=CARTESIAN_POINT('Ctrl Pts',(1.32288534609529,-1.44429727432079,29.));
#23538=CARTESIAN_POINT('Ctrl Pts',(1.3099943443598,-1.45858831293731,29.));
#23539=CARTESIAN_POINT('Ctrl Pts',(1.29691491924979,-1.47268731356655,29.));
#23540=CARTESIAN_POINT('Ctrl Pts',(1.24603363784778,-1.52753492441104,29.));
#23541=CARTESIAN_POINT('Ctrl Pts',(1.19225580967216,-1.57953769268553,29.));
#23542=CARTESIAN_POINT('Ctrl Pts',(1.1358667874795,-1.62843129863239,29.));
#23543=CARTESIAN_POINT('Ctrl Pts',(1.09369930723698,-1.6649937372522,29.));
#23544=CARTESIAN_POINT('Ctrl Pts',(1.05007049363608,-1.69981733826376,29.));
#23545=CARTESIAN_POINT('Ctrl Pts',(1.00508328076865,-1.73278182943765,29.));
#23546=CARTESIAN_POINT('Ctrl Pts',(0.991019284017403,-1.74308725774107,
29.));
#23547=CARTESIAN_POINT('Ctrl Pts',(0.976822434853456,-1.75321091355829,
29.));
#23548=CARTESIAN_POINT('Ctrl Pts',(0.962495636971034,-1.76314889540177,
29.));
#23549=CARTESIAN_POINT('Ctrl Pts',(0.948702692966066,-1.77271656210681,
29.));
#23550=CARTESIAN_POINT('Ctrl Pts',(0.934796339602229,-1.78210719109177,
29.));
#23551=CARTESIAN_POINT('Ctrl Pts',(0.920784555255717,-1.79131455083345,
29.));
#23552=CARTESIAN_POINT('Ctrl Pts',(0.857822233634552,-1.83268806408493,
29.));
#23553=CARTESIAN_POINT('Ctrl Pts',(0.792703365228481,-1.87038503190709,
29.));
#23554=CARTESIAN_POINT('Ctrl Pts',(0.725689641419005,-1.90412588607056,
29.));
#23555=CARTESIAN_POINT('Ctrl Pts',(0.674455559543145,-1.92992182138804,
29.));
#23556=CARTESIAN_POINT('Ctrl Pts',(0.622112945371267,-1.95340496957484,
29.));
#23557=CARTESIAN_POINT('Ctrl Pts',(0.568764876142657,-1.97443513991583,
29.));
#23558=CARTESIAN_POINT('Ctrl Pts',(0.556316873757165,-1.97934222679559,
29.));
#23559=CARTESIAN_POINT('Ctrl Pts',(0.543814084655739,-1.98411569285989,
29.));
#23560=CARTESIAN_POINT('Ctrl Pts',(0.531258445741635,-1.98875612844697,
29.));
#23561=CARTESIAN_POINT('Ctrl Pts',(-1.66729377121886,-0.00130306451899955,
27.8714803633902));
#23562=CARTESIAN_POINT('Ctrl Pts',(-1.66802804256299,-0.0867857428702756,
27.8772098489549));
#23563=CARTESIAN_POINT('Ctrl Pts',(-1.66202149744119,-0.172164864355061,
27.8829393345197));
#23564=CARTESIAN_POINT('Ctrl Pts',(-1.64891509598314,-0.256439697376359,
27.8886688200844));
#23565=CARTESIAN_POINT('Ctrl Pts',(-1.56417477952568,-0.801324274770393,
27.9257131927483));
#23566=CARTESIAN_POINT('Ctrl Pts',(-1.18263521873075,-1.30004566716866,
27.9627575654121));
#23567=CARTESIAN_POINT('Ctrl Pts',(-0.678896970418698,-1.52439134880859,
27.999801938076));
#23568=CARTESIAN_POINT('Ctrl Pts',(-0.175158722106646,-1.74873703044852,
28.0368463107398));
#23569=CARTESIAN_POINT('Ctrl Pts',(0.450778213722533,-1.69870700133011,
28.0738906834037));
#23570=CARTESIAN_POINT('Ctrl Pts',(0.912473825127841,-1.39717253420635,
28.1109350560675));
#23571=CARTESIAN_POINT('Ctrl Pts',(1.37416943653315,-1.09563806708259,28.1479794287314));
#23572=CARTESIAN_POINT('Ctrl Pts',(1.67162372351458,-0.542599161953481,
28.1850238013952));
#23573=CARTESIAN_POINT('Ctrl Pts',(1.66871373497161,0.0088176010985061,
28.2220681740591));
#23574=CARTESIAN_POINT('Ctrl Pts',(1.66580374642864,0.560234364150496,28.2591125467229));
#23575=CARTESIAN_POINT('Ctrl Pts',(1.36252948236125,1.11002898512537,28.2961569193868));
#23576=CARTESIAN_POINT('Ctrl Pts',(0.897679091078753,1.40669133067121,28.3332012920506));
#23577=CARTESIAN_POINT('Ctrl Pts',(0.432828699796255,1.70335367621706,28.3702456647145));
#23578=CARTESIAN_POINT('Ctrl Pts',(-0.193597818701355,1.74688374633388,
28.4072900373784));
#23579=CARTESIAN_POINT('Ctrl Pts',(-0.69494282889168,1.51719457203667,28.4443344100422));
#23580=CARTESIAN_POINT('Ctrl Pts',(-1.196287839082,1.28750539773946,28.4813787827061));
#23581=CARTESIAN_POINT('Ctrl Pts',(-1.57255134096505,0.784596979028224,
28.5184231553699));
#23582=CARTESIAN_POINT('Ctrl Pts',(-1.65153326697391,0.238931147268006,
28.5554675280338));
#23583=CARTESIAN_POINT('Ctrl Pts',(-1.66291353417212,0.160307805445838,
28.5608051398193));
#23584=CARTESIAN_POINT('Ctrl Pts',(-1.66812192138366,0.0807967744989645,
28.5661427516047));
#23585=CARTESIAN_POINT('Ctrl Pts',(-1.66745735078673,0.00120170187390745,
28.5714803633902));
#23586=CARTESIAN_POINT('Ctrl Pts',(-0.530170217188634,-1.98517432567172,
29.));
#23587=CARTESIAN_POINT('Ctrl Pts',(-1.19025956241812,-1.80888768575368,
28.9629556273361));
#23588=CARTESIAN_POINT('Ctrl Pts',(-2.30934991790679,-0.749104679977639,
28.8888668820084));
#23589=CARTESIAN_POINT('Ctrl Pts',(-1.88125738141003,1.53835568783795,28.7777337640169));
#23590=CARTESIAN_POINT('Ctrl Pts',(0.271806531570387,2.41264813750898,28.6666006460253));
#23591=CARTESIAN_POINT('Ctrl Pts',(2.17449559304179,1.08136903079269,28.5554675280338));
#23592=CARTESIAN_POINT('Ctrl Pts',(2.08783197155072,-1.24094928383581,28.4443344100422));
#23593=CARTESIAN_POINT('Ctrl Pts',(0.0898704340492965,-2.42681281153263,
28.3332012920506));
#23594=CARTESIAN_POINT('Ctrl Pts',(-1.99011943914583,-1.39192006204976,
28.2220681740591));
#23595=CARTESIAN_POINT('Ctrl Pts',(-2.24879050981126,0.917099090480224,
28.1109350560675));
#23596=CARTESIAN_POINT('Ctrl Pts',(-0.449219217968869,2.38665611117453,
27.999801938076));
#23597=CARTESIAN_POINT('Ctrl Pts',(1.76146356868064,1.6719019509933,27.8886688200844));
#23598=CARTESIAN_POINT('Ctrl Pts',(2.36000201199169,-0.573068912759941,
27.7775357020928));
#23599=CARTESIAN_POINT('Ctrl Pts',(0.798565170672349,-2.29353090612058,
27.6664025841013));
#23600=CARTESIAN_POINT('Ctrl Pts',(-1.49374549619868,-1.91487023989728,
27.5552694661097));
#23601=CARTESIAN_POINT('Ctrl Pts',(-2.4189238064285,0.216358730773912,27.4441363481182));
#23602=CARTESIAN_POINT('Ctrl Pts',(-1.13020663702663,2.14956575456656,27.3330032301266));
#23603=CARTESIAN_POINT('Ctrl Pts',(1.19291950474651,2.1154065927935,27.2218701121351));
#23604=CARTESIAN_POINT('Ctrl Pts',(2.42423908872827,0.145143535993706,27.1107369941435));
#23605=CARTESIAN_POINT('Ctrl Pts',(1.43679947210715,-1.95796032739892,26.999603876152));
#23606=CARTESIAN_POINT('Ctrl Pts',(-0.865655485103571,-2.26906197521519,
26.8884707581604));
#23607=CARTESIAN_POINT('Ctrl Pts',(-2.37582851633814,-0.503428720754339,
26.7773376401688));
#23608=CARTESIAN_POINT('Ctrl Pts',(-1.71154975386622,1.72296227565052,26.6662045221772));
#23609=CARTESIAN_POINT('Ctrl Pts',(0.51920669687721,2.37243040203942,26.5550714041857));
#23610=CARTESIAN_POINT('Ctrl Pts',(2.27476474931693,0.850556836234861,26.4439382861941));
#23611=CARTESIAN_POINT('Ctrl Pts',(1.9483685659561,-1.44977981832677,26.3328051682026));
#23612=CARTESIAN_POINT('Ctrl Pts',(-0.161251214260656,-2.42322092316419,
26.221672050211));
#23613=CARTESIAN_POINT('Ctrl Pts',(-2.12328753730864,-1.17883486062637,
26.1105389322195));
#23614=CARTESIAN_POINT('Ctrl Pts',(-2.14200753395606,1.14446726409082,25.9994058142279));
#23615=CARTESIAN_POINT('Ctrl Pts',(-0.200277927177756,2.42030790331167,
25.8882726962363));
#23616=CARTESIAN_POINT('Ctrl Pts',(1.92475392154391,1.48098748682692,25.7771395782448));
#23617=CARTESIAN_POINT('Ctrl Pts',(2.28817522362595,-0.813790968595164,
25.6660064602532));
#23618=CARTESIAN_POINT('Ctrl Pts',(0.557368499380946,-2.36375589911376,
25.5548733422617));
#23619=CARTESIAN_POINT('Ctrl Pts',(-1.68356381332587,-1.75031839420915,
25.4437402242701));
#23620=CARTESIAN_POINT('Ctrl Pts',(-2.38363225964151,0.465079396921421,
25.3326071062785));
#23621=CARTESIAN_POINT('Ctrl Pts',(-0.902106643086596,2.25481821865058,
25.221473988287));
#23622=CARTESIAN_POINT('Ctrl Pts',(1.40506247979517,1.98085865788643,25.1103408702954));
#23623=CARTESIAN_POINT('Ctrl Pts',(2.42626311844678,-0.106060712410309,
24.9992077523039));
#23624=CARTESIAN_POINT('Ctrl Pts',(1.22685225431082,-2.09590914420127,24.8880746343123));
#23625=CARTESIAN_POINT('Ctrl Pts',(-1.09542208140494,-2.16749903303861,
24.7769415163207));
#23626=CARTESIAN_POINT('Ctrl Pts',(-2.41512301282573,-0.255308494908708,
24.6658083983292));
#23627=CARTESIAN_POINT('Ctrl Pts',(-1.52440830459303,1.89055042660624,24.5546752803376));
#23628=CARTESIAN_POINT('Ctrl Pts',(0.761504884129454,2.30610318635139,24.4435421623461));
#23629=CARTESIAN_POINT('Ctrl Pts',(2.35045883035646,0.611019542610869,24.3324090443546));
#23630=CARTESIAN_POINT('Ctrl Pts',(1.7881803418832,-1.64329323602198,24.2212759263629));
#23631=CARTESIAN_POINT('Ctrl Pts',(-0.410711177573986,-2.39359936565602,
24.1101428083714));
#23632=CARTESIAN_POINT('Ctrl Pts',(-2.23370366188104,-0.953189144688686,
23.9990096903798));
#23633=CARTESIAN_POINT('Ctrl Pts',(-2.01232263711515,1.35961729865687,23.8878765723883));
#23634=CARTESIAN_POINT('Ctrl Pts',(0.0508152693856986,2.42804847625626,
23.7767434543967));
#23635=CARTESIAN_POINT('Ctrl Pts',(2.06744504127525,1.27423412132916,23.6656103364052));
#23636=CARTESIAN_POINT('Ctrl Pts',(2.19186773754582,-1.04580945480468,23.5544772184136));
#23637=CARTESIAN_POINT('Ctrl Pts',(0.310206809340991,-2.40868705524225,
23.443344100422));
#23638=CARTESIAN_POINT('Ctrl Pts',(-1.85536760039376,-1.56703945772346,
23.3322109824305));
#23639=CARTESIAN_POINT('Ctrl Pts',(-2.322836555691,0.708824329575872,23.2210778644389));
#23640=CARTESIAN_POINT('Ctrl Pts',(-0.664354069263913,2.33594419139362,
23.1099447464474));
#23641=CARTESIAN_POINT('Ctrl Pts',(1.60217141007485,1.82511598738049,22.9988116284558));
#23642=CARTESIAN_POINT('Ctrl Pts',(2.40232655406092,-0.356130204148507,
22.8876785104642));
#23643=CARTESIAN_POINT('Ctrl Pts',(1.00377788111867,-2.21143201569255,22.7765453924727));
#23644=CARTESIAN_POINT('Ctrl Pts',(-1.3134678169358,-2.04274420535881,22.6654122744811));
#23645=CARTESIAN_POINT('Ctrl Pts',(-2.42857607134113,-0.00445649665224475,
22.5542791564896));
#23646=CARTESIAN_POINT('Ctrl Pts',(-1.32095591743234,2.03790997319645,22.443146038498));
#23647=CARTESIAN_POINT('Ctrl Pts',(0.995655084428766,2.21510102422083,22.3320129205065));
#23648=CARTESIAN_POINT('Ctrl Pts',(2.40100336441846,0.364944432351608,22.2208798025149));
#23649=CARTESIAN_POINT('Ctrl Pts',(1.60885886272077,-1.81922366807872,22.1097466845233));
#23650=CARTESIAN_POINT('Ctrl Pts',(-0.655776594206566,-2.33836666353754,
21.9986135665318));
#23651=CARTESIAN_POINT('Ctrl Pts',(-2.32021950100116,-0.717344451311874,
21.8874804485402));
#23652=CARTESIAN_POINT('Ctrl Pts',(-1.86110619752919,1.56021963715706,21.7763473305487));
#23653=CARTESIAN_POINT('Ctrl Pts',(0.301364750346359,2.40980930405301,21.6652142125571));
#23654=CARTESIAN_POINT('Ctrl Pts',(2.18801481710634,1.05384664671037,21.5540810945656));
#23655=CARTESIAN_POINT('Ctrl Pts',(2.07210760382199,-1.2666379407027,21.442947976574));
#23656=CARTESIAN_POINT('Ctrl Pts',(0.0597259541680415,-2.42784563039867,
21.3318148585825));
#23657=CARTESIAN_POINT('Ctrl Pts',(-2.00731923954813,-1.36699344008564,
21.2206817405908));
#23658=CARTESIAN_POINT('Ctrl Pts',(-2.23718685788182,0.944984950940279,
21.1095486225994));
#23659=CARTESIAN_POINT('Ctrl Pts',(-0.419493009128206,2.39207592060309,
20.9984155046077));
#23660=CARTESIAN_POINT('Ctrl Pts',(1.7821373527842,1.64984485657254,20.8872823866162));
#23661=CARTESIAN_POINT('Ctrl Pts',(2.35268546495377,-0.602389157518069,
20.7761492686246));
#23662=CARTESIAN_POINT('Ctrl Pts',(0.769963239246222,-2.30329290471873,
20.6650161506331));
#23663=CARTESIAN_POINT('Ctrl Pts',(-1.51745964933489,-1.89613232903235,
20.5538830326415));
#23664=CARTESIAN_POINT('Ctrl Pts',(-2.41604373856618,0.24644318568101,20.44274991465));
#23665=CARTESIAN_POINT('Ctrl Pts',(-1.10336950687639,2.16346419607446,20.3316167966584));
#23666=CARTESIAN_POINT('Ctrl Pts',(1.21915193180051,2.10039762278245,20.2204836786668));
#23667=CARTESIAN_POINT('Ctrl Pts',(2.42585752542742,0.114964471039976,20.1093505606753));
#23668=CARTESIAN_POINT('Ctrl Pts',(1.41232285348001,-1.97568868333651,19.9982174426837));
#23669=CARTESIAN_POINT('Ctrl Pts',(-0.893825325748239,-2.2581138043306,
19.8870843246922));
#23670=CARTESIAN_POINT('Ctrl Pts',(-2.38190930300825,-0.4738242701237,19.7759512067006));
#23671=CARTESIAN_POINT('Ctrl Pts',(-1.68997629510449,1.74412784145651,19.6648180887091));
#23672=CARTESIAN_POINT('Ctrl Pts',(0.548689842456826,2.36578558927548,19.5536849707175));
#23673=CARTESIAN_POINT('Ctrl Pts',(2.28517284872419,0.82218308608128,19.4425518527259));
#23674=CARTESIAN_POINT('Ctrl Pts',(1.93017685695003,-1.47391342438527,19.3314187347344));
#23675=CARTESIAN_POINT('Ctrl Pts',(-0.191395150412758,-2.42102695967158,
19.2202856167428));
#23676=CARTESIAN_POINT('Ctrl Pts',(-2.13779058223796,-1.15232017062793,
19.1091524987513));
#23677=CARTESIAN_POINT('Ctrl Pts',(-2.12760400594706,1.17103316317459,18.9980193807597));
#23678=CARTESIAN_POINT('Ctrl Pts',(-0.170134977547301,2.42261514214274,
18.8868862627681));
#23679=CARTESIAN_POINT('Ctrl Pts',(1.9430184348445,1.45691614743391,18.7757531447766));
#23680=CARTESIAN_POINT('Ctrl Pts',(2.27790227156009,-0.842194003777161,
18.664620026785));
#23681=CARTESIAN_POINT('Ctrl Pts',(0.52784999826971,-2.37052551568832,18.5534869087934));
#23682=CARTESIAN_POINT('Ctrl Pts',(-1.70509933605923,-1.72920021145774,
18.4423537908019));
#23683=CARTESIAN_POINT('Ctrl Pts',(-2.37788229208364,0.494644591072267,
18.3312206728103));
#23684=CARTESIAN_POINT('Ctrl Pts',(-0.873549834886296,2.26598780907704,
18.2200875548188));
#23685=CARTESIAN_POINT('Ctrl Pts',(1.42878011639417,1.96299190141644,18.1089544368272));
#23686=CARTESIAN_POINT('Ctrl Pts',(2.42636094490168,-0.135794412509918,
17.9978213188357));
#23687=CARTESIAN_POINT('Ctrl Pts',(1.19738788458608,-2.11199363605741,17.8866882008441));
#23688=CARTESIAN_POINT('Ctrl Pts',(-0.343660854083971,-2.13791714127778,
17.8125994555164));
#23689=CARTESIAN_POINT('Ctrl Pts',(-0.949553552261494,-1.82218155349229,
17.7755550828525));
#23690=CARTESIAN_POINT('Ctrl Pts',(-0.496734897087716,-1.85997880000276,
29.0748149723825));
#23691=CARTESIAN_POINT('Ctrl Pts',(-1.11519553923768,-1.69480972203762,
29.0377705997186));
#23692=CARTESIAN_POINT('Ctrl Pts',(-2.16371017575061,-0.70186220208636,
28.9636818543909));
#23693=CARTESIAN_POINT('Ctrl Pts',(-1.76261540436122,1.441338893638,28.8525487363994));
#23694=CARTESIAN_POINT('Ctrl Pts',(0.254664983263946,2.26049386676127,28.7414156184078));
#23695=CARTESIAN_POINT('Ctrl Pts',(2.03736047331189,1.01317221678926,28.6302825004163));
#23696=CARTESIAN_POINT('Ctrl Pts',(1.95616231523563,-1.16268850043293,28.5191493824247));
#23697=CARTESIAN_POINT('Ctrl Pts',(0.0842027321818088,-2.27376524200133,
28.4080162644332));
#23698=CARTESIAN_POINT('Ctrl Pts',(-1.86461204863313,-1.30413826797557,
28.2968831464416));
#23699=CARTESIAN_POINT('Ctrl Pts',(-2.1069699621876,0.859262002201165,28.18575002845));
#23700=CARTESIAN_POINT('Ctrl Pts',(-0.42088909330076,2.23614103420343,28.0746169104585));
#23701=CARTESIAN_POINT('Ctrl Pts',(1.65037641901529,1.56646302761273,27.9634837924669));
#23702=CARTESIAN_POINT('Ctrl Pts',(2.21116788259043,-0.536928175470663,
27.8523506744754));
#23703=CARTESIAN_POINT('Ctrl Pts',(0.748203454308011,-2.14888879398133,
27.7412175564837));
#23704=CARTESIAN_POINT('Ctrl Pts',(-1.39954205512358,-1.79410845934652,
27.6300844384923));
#23705=CARTESIAN_POINT('Ctrl Pts',(-2.26637375901817,0.202714012180677,
27.5189513205007));
#23706=CARTESIAN_POINT('Ctrl Pts',(-1.05892986691768,2.01400284146476,27.4078182025091));
#23707=CARTESIAN_POINT('Ctrl Pts',(1.11768773162403,1.98199793594985,27.2966850845176));
#23708=CARTESIAN_POINT('Ctrl Pts',(2.27135383168271,0.135990021840718,27.185551966526));
#23709=CARTESIAN_POINT('Ctrl Pts',(1.34618734657985,-1.83448105947885,27.0744188485344));
#23710=CARTESIAN_POINT('Ctrl Pts',(-0.811062700931283,-2.12596300245047,
26.9632857305429));
#23711=CARTESIAN_POINT('Ctrl Pts',(-2.22599628439971,-0.47167985995323,
26.8521526125513));
#23712=CARTESIAN_POINT('Ctrl Pts',(-1.60361043167528,1.61430321985961,26.7410194945598));
#23713=CARTESIAN_POINT('Ctrl Pts',(0.486462793983747,2.22281247304678,26.6298863765682));
#23714=CARTESIAN_POINT('Ctrl Pts',(2.13130612964755,0.796916252208208,26.5187532585767));
#23715=CARTESIAN_POINT('Ctrl Pts',(1.82549420492022,-1.35834908395122,26.4076201405851));
#23716=CARTESIAN_POINT('Ctrl Pts',(-0.151081865265427,-2.27039987698986,
26.2964870225935));
#23717=CARTESIAN_POINT('Ctrl Pts',(-1.98938186668712,-1.10449133918118,
26.185353904602));
#23718=CARTESIAN_POINT('Ctrl Pts',(-2.0069212819667,1.07229114389529,26.0742207866104));
#23719=CARTESIAN_POINT('Ctrl Pts',(-0.187647348568785,2.26767056747804,
25.9630876686188));
#23720=CARTESIAN_POINT('Ctrl Pts',(1.80336882408676,1.38758863287,25.8519545506273));
#23721=CARTESIAN_POINT('Ctrl Pts',(2.14387086897055,-0.762469033397635,
25.7408214326357));
#23722=CARTESIAN_POINT('Ctrl Pts',(0.522217912669773,-2.21468502986276,
25.6296883146442));
#23723=CARTESIAN_POINT('Ctrl Pts',(-1.57738943161999,-1.63993411781724,
25.5185551966526));
#23724=CARTESIAN_POINT('Ctrl Pts',(-2.23330788263933,0.435749046018521,
25.407422078661));
#23725=CARTESIAN_POINT('Ctrl Pts',(-0.845215057330029,2.11261753203009,
25.2962889606695));
#23726=CARTESIAN_POINT('Ctrl Pts',(1.31645185579057,1.85593530090815,25.1851558426779));
#23727=CARTESIAN_POINT('Ctrl Pts',(2.27325021545028,-0.0993719665045596,
25.0740227246864));
#23728=CARTESIAN_POINT('Ctrl Pts',(1.14948050367395,-1.96373009893084,24.9628896066948));
#23729=CARTESIAN_POINT('Ctrl Pts',(-1.02633900817686,-2.03080515315156,
24.8517564887032));
#23730=CARTESIAN_POINT('Ctrl Pts',(-2.26281266343432,-0.239207399496329,
24.7406233707117));
#23731=CARTESIAN_POINT('Ctrl Pts',(-1.42827110567824,1.77132238128959,24.6294902527201));
#23732=CARTESIAN_POINT('Ctrl Pts',(0.713480384197537,2.16066820014965,24.5183571347286));
#23733=CARTESIAN_POINT('Ctrl Pts',(2.20222654414142,0.572485439161143,24.407224016737));
#23734=CARTESIAN_POINT('Ctrl Pts',(1.67540829209497,-1.53965852855496,24.2960908987454));
#23735=CARTESIAN_POINT('Ctrl Pts',(-0.384809572304588,-2.24264641056841,
24.1849577807539));
#23736=CARTESIAN_POINT('Ctrl Pts',(-2.09283457017381,-0.893076027927082,
24.0738246627623));
#23737=CARTESIAN_POINT('Ctrl Pts',(-1.88541499625397,1.27387268660304,23.9626915447708));
#23738=CARTESIAN_POINT('Ctrl Pts',(0.0476105914486115,2.2749229792137,23.8515584267792));
#23739=CARTESIAN_POINT('Ctrl Pts',(1.93706109192281,1.19387422115205,23.7404253087876));
#23740=CARTESIAN_POINT('Ctrl Pts',(2.05363703908762,-0.979855214539392,
23.6292921907961));
#23741=CARTESIAN_POINT('Ctrl Pts',(0.290643537713249,-2.25678259115896,
23.5181590728045));
#23742=CARTESIAN_POINT('Ctrl Pts',(-1.73835836899447,-1.46821371425264,
23.407025954813));
#23743=CARTESIAN_POINT('Ctrl Pts',(-2.17634627527977,0.664122142266367,
23.2958928368214));
#23744=CARTESIAN_POINT('Ctrl Pts',(-0.622456410274362,2.18862727459039,
23.1847597188299));
#23745=CARTESIAN_POINT('Ctrl Pts',(1.5011300610597,1.7100145816792,23.0736266008383));
#23746=CARTESIAN_POINT('Ctrl Pts',(2.25082321660849,-0.333670761902858,
22.9624934828467));
#23747=CARTESIAN_POINT('Ctrl Pts',(0.940474372778667,-2.07196749103822,
22.8513603648552));
#23748=CARTESIAN_POINT('Ctrl Pts',(-1.23063363372879,-1.91391802052963,
22.7402272468636));
#23749=CARTESIAN_POINT('Ctrl Pts',(-2.27541730137984,-0.00417544655311686,
22.629094128872));
#23750=CARTESIAN_POINT('Ctrl Pts',(-1.23764949525578,1.90938866045279,22.5179610108805));
#23751=CARTESIAN_POINT('Ctrl Pts',(0.93286384233578,2.07540511260695,22.4068278928889));
#23752=CARTESIAN_POINT('Ctrl Pts',(2.24958347425864,0.341929118554036,22.2956947748974));
#23753=CARTESIAN_POINT('Ctrl Pts',(1.50739576779718,-1.70449386299853,22.1845616569058));
#23754=CARTESIAN_POINT('Ctrl Pts',(-0.614419875871358,-2.1908969729101,
22.0734285389143));
#23755=CARTESIAN_POINT('Ctrl Pts',(-2.1738942658121,-0.672104940349877,
21.9622954209227));
#23756=CARTESIAN_POINT('Ctrl Pts',(-1.74373506003647,1.46182398741138,21.8511623029312));
#23757=CARTESIAN_POINT('Ctrl Pts',(0.282359105426515,2.25783406506196,21.7400291849396));
#23758=CARTESIAN_POINT('Ctrl Pts',(2.05002710405932,0.987385538885627,21.628896066948));
#23759=CARTESIAN_POINT('Ctrl Pts',(1.94142960877218,-1.18675709559613,21.5177629489565));
#23760=CARTESIAN_POINT('Ctrl Pts',(0.0559593216202335,-2.2747329258819,
21.4066298309649));
#23761=CARTESIAN_POINT('Ctrl Pts',(-1.8807271392319,-1.28078364978945,21.2954967129733));
#23762=CARTESIAN_POINT('Ctrl Pts',(-2.09609809752954,0.885389233751969,
21.1843635949818));
#23763=CARTESIAN_POINT('Ctrl Pts',(-0.393037575409816,2.24121904196669,
21.0732304769902));
#23764=CARTESIAN_POINT('Ctrl Pts',(1.66974640564629,1.54579696948286,20.9620973589987));
#23765=CARTESIAN_POINT('Ctrl Pts',(2.20431275545938,-0.564399331507581,
20.8509642410071));
#23766=CARTESIAN_POINT('Ctrl Pts',(0.721405310989425,-2.15803514964562,
20.7398311230156));
#23767=CARTESIAN_POINT('Ctrl Pts',(-1.42176066913796,-1.77655225961412,
20.628698005024));
#23768=CARTESIAN_POINT('Ctrl Pts',(-2.26367532337088,0.230901183258412,
20.5175648870324));
#23769=CARTESIAN_POINT('Ctrl Pts',(-1.03378522723196,2.02702477421066,20.4064317690409));
#23770=CARTESIAN_POINT('Ctrl Pts',(1.14226580396866,1.96793551046437,20.2952986510493));
#23771=CARTESIAN_POINT('Ctrl Pts',(2.27287020125823,0.107714207323098,20.1841655330578));
#23772=CARTESIAN_POINT('Ctrl Pts',(1.32325435215538,-1.85109137212314,20.0730324150662));
#23773=CARTESIAN_POINT('Ctrl Pts',(-0.837456003383859,-2.11570528075782,
19.9618992970746));
#23774=CARTESIAN_POINT('Ctrl Pts',(-2.23169358470602,-0.443942421559709,
19.8507661790831));
#23775=CARTESIAN_POINT('Ctrl Pts',(-1.58339750859812,1.63413397385441,19.7396330610915));
#23776=CARTESIAN_POINT('Ctrl Pts',(0.514086577460258,2.21658671709625,19.6284999431));
#23777=CARTESIAN_POINT('Ctrl Pts',(2.14105783960848,0.770331899851958,19.5173668251084));
#23778=CARTESIAN_POINT('Ctrl Pts',(1.80844976068701,-1.38096069798226,19.4062337071169));
#23779=CARTESIAN_POINT('Ctrl Pts',(-0.179324766388269,-2.26834427636504,
19.2951005891253));
#23780=CARTESIAN_POINT('Ctrl Pts',(-2.00297027338529,-1.07964880487677,
19.1839674711338));
#23781=CARTESIAN_POINT('Ctrl Pts',(-1.99342611612885,1.097181657771,19.0728343531422));
#23782=CARTESIAN_POINT('Ctrl Pts',(-0.159405371752351,2.26983229970319,
18.9617012351506));
#23783=CARTESIAN_POINT('Ctrl Pts',(1.82048148119308,1.36503535864129,18.850568117159));
#23784=CARTESIAN_POINT('Ctrl Pts',(2.13424578324943,-0.789080823914506,
18.7394349991675));
#23785=CARTESIAN_POINT('Ctrl Pts',(0.494561003367273,-2.22102771883975,
18.6283018811759));
#23786=CARTESIAN_POINT('Ctrl Pts',(-1.5975668111141,-1.62014775865258,18.5171687631844));
#23787=CARTESIAN_POINT('Ctrl Pts',(-2.22792053825349,0.463449703652169,
18.4060356451928));
#23788=CARTESIAN_POINT('Ctrl Pts',(-0.818459191529514,2.12308270938467,
18.2949025272012));
#23789=CARTESIAN_POINT('Ctrl Pts',(1.33867373358228,1.83919531599638,18.1837694092097));
#23790=CARTESIAN_POINT('Ctrl Pts',(2.27334187245483,-0.127230503216293,
18.0726362912181));
#23791=CARTESIAN_POINT('Ctrl Pts',(1.12187431194823,-1.97880021820166,17.9615031732266));
#23792=CARTESIAN_POINT('Ctrl Pts',(-0.321987794583605,-2.00308885094696,
17.8874144278989));
#23793=CARTESIAN_POINT('Ctrl Pts',(-0.889669715064486,-1.70726520861333,
17.850370055235));
#23794=CARTESIAN_POINT('Ctrl Pts',(-0.463299576986798,-1.7347832743338,
29.149629944765));
#23795=CARTESIAN_POINT('Ctrl Pts',(-1.04013151605724,-1.58073175832155,
29.1125855721011));
#23796=CARTESIAN_POINT('Ctrl Pts',(-2.01807043359442,-0.654619724195083,
29.0384968267734));
#23797=CARTESIAN_POINT('Ctrl Pts',(-1.64397342731241,1.34432209943806,28.9273637087818));
#23798=CARTESIAN_POINT('Ctrl Pts',(0.237523434957504,2.10833959601355,28.8162305907903));
#23799=CARTESIAN_POINT('Ctrl Pts',(1.900225353582,0.944975402785826,28.7050974727987));
#23800=CARTESIAN_POINT('Ctrl Pts',(1.82449265892053,-1.08442771703006,28.5939643548072));
#23801=CARTESIAN_POINT('Ctrl Pts',(0.0785350303143197,-2.12071767247004,
28.4828312368156));
#23802=CARTESIAN_POINT('Ctrl Pts',(-1.73910465812042,-1.21635647390137,
28.3716981188241));
#23803=CARTESIAN_POINT('Ctrl Pts',(-1.96514941456394,0.801424913922105,
28.2605650008325));
#23804=CARTESIAN_POINT('Ctrl Pts',(-0.392558968632649,2.08562595723233,
28.149431882841));
#23805=CARTESIAN_POINT('Ctrl Pts',(1.53928926934995,1.46102410423217,28.0382987648494));
#23806=CARTESIAN_POINT('Ctrl Pts',(2.06233375318916,-0.500787438181385,
27.9271656468578));
#23807=CARTESIAN_POINT('Ctrl Pts',(0.697841737943671,-2.00424668184208,
27.8160325288663));
#23808=CARTESIAN_POINT('Ctrl Pts',(-1.30533861404847,-1.67334667879575,
27.7048994108747));
#23809=CARTESIAN_POINT('Ctrl Pts',(-2.11382371160785,0.189069293587439,
27.5937662928831));
#23810=CARTESIAN_POINT('Ctrl Pts',(-0.98765309680873,1.87843992836297,27.4826331748916));
#23811=CARTESIAN_POINT('Ctrl Pts',(1.04245595850156,1.8485892791062,27.3715000569));
#23812=CARTESIAN_POINT('Ctrl Pts',(2.11846857463714,0.126836507687731,27.2603669389085));
#23813=CARTESIAN_POINT('Ctrl Pts',(1.25557522105255,-1.71100179155877,27.1492338209169));
#23814=CARTESIAN_POINT('Ctrl Pts',(-0.756469916759,-1.98286402968576,27.0381007029254));
#23815=CARTESIAN_POINT('Ctrl Pts',(-2.07616405246128,-0.439930999152115,
26.9269675849338));
#23816=CARTESIAN_POINT('Ctrl Pts',(-1.49567110948434,1.50564416406869,26.8158344669423));
#23817=CARTESIAN_POINT('Ctrl Pts',(0.453718891090288,2.07319454405416,26.7047013489507));
#23818=CARTESIAN_POINT('Ctrl Pts',(1.98784750997817,0.743275668181553,26.5935682309591));
#23819=CARTESIAN_POINT('Ctrl Pts',(1.70261984388434,-1.26691834957566,26.4824351129675));
#23820=CARTESIAN_POINT('Ctrl Pts',(-0.140912516270202,-2.11757883081554,
26.371301994976));
#23821=CARTESIAN_POINT('Ctrl Pts',(-1.85547619606559,-1.03014781773599,
26.2601688769844));
#23822=CARTESIAN_POINT('Ctrl Pts',(-1.87183502997734,1.00011502369975,26.1490357589929));
#23823=CARTESIAN_POINT('Ctrl Pts',(-0.175016769959812,2.11503323164442,
26.0379026410014));
#23824=CARTESIAN_POINT('Ctrl Pts',(1.68198372662962,1.29418977891308,25.9267695230097));
#23825=CARTESIAN_POINT('Ctrl Pts',(1.99956651431514,-0.711147098200105,
25.8156364050183));
#23826=CARTESIAN_POINT('Ctrl Pts',(0.4870673259586,-2.06561416061176,25.7045032870266));
#23827=CARTESIAN_POINT('Ctrl Pts',(-1.47121504991412,-1.52954984142534,
25.5933701690351));
#23828=CARTESIAN_POINT('Ctrl Pts',(-2.08298350563717,0.406418695115622,
25.4822370510435));
#23829=CARTESIAN_POINT('Ctrl Pts',(-0.788323471573461,1.97041684540958,
25.371103933052));
#23830=CARTESIAN_POINT('Ctrl Pts',(1.22784123178597,1.73101194392987,25.2599708150604));
#23831=CARTESIAN_POINT('Ctrl Pts',(2.12023731245378,-0.0926832205988131,
25.1488376970689));
#23832=CARTESIAN_POINT('Ctrl Pts',(1.07210875303708,-1.83155105366041,25.0377045790773));
#23833=CARTESIAN_POINT('Ctrl Pts',(-0.957255934948788,-1.89411127326451,
24.9265714610857));
#23834=CARTESIAN_POINT('Ctrl Pts',(-2.11050231404291,-0.223106304083948,
24.8154383430942));
#23835=CARTESIAN_POINT('Ctrl Pts',(-1.33213390676344,1.65209433597293,24.7043052251026));
#23836=CARTESIAN_POINT('Ctrl Pts',(0.665455884265618,2.0152332139479,24.5931721071111));
#23837=CARTESIAN_POINT('Ctrl Pts',(2.05399425792638,0.533951335711417,24.4820389891195));
#23838=CARTESIAN_POINT('Ctrl Pts',(1.56263624230674,-1.43602382108795,24.370905871128));
#23839=CARTESIAN_POINT('Ctrl Pts',(-0.358907967035191,-2.09169345548081,
24.2597727531364));
#23840=CARTESIAN_POINT('Ctrl Pts',(-1.95196547846659,-0.832962911165477,
24.1486396351448));
#23841=CARTESIAN_POINT('Ctrl Pts',(-1.75850735539279,1.1881280745492,24.0375065171533));
#23842=CARTESIAN_POINT('Ctrl Pts',(0.0444059135115228,2.12179748217114,
23.9263733991617));
#23843=CARTESIAN_POINT('Ctrl Pts',(1.80667714257038,1.11351432097495,23.8152402811702));
#23844=CARTESIAN_POINT('Ctrl Pts',(1.91540634062942,-0.9139009742741,23.7041071631786));
#23845=CARTESIAN_POINT('Ctrl Pts',(0.271080266085507,-2.10487812707567,
23.592974045187));
#23846=CARTESIAN_POINT('Ctrl Pts',(-1.62134913759518,-1.36938797078182,
23.4818409271955));
#23847=CARTESIAN_POINT('Ctrl Pts',(-2.02985599486855,0.619419954956861,
23.3707078092039));
#23848=CARTESIAN_POINT('Ctrl Pts',(-0.580558751284808,2.04131035778717,
23.2595746912124));
#23849=CARTESIAN_POINT('Ctrl Pts',(1.40008871204456,1.59491317597791,23.1484415732208));
#23850=CARTESIAN_POINT('Ctrl Pts',(2.09931987915605,-0.311211319657211,
23.0373084552292));
#23851=CARTESIAN_POINT('Ctrl Pts',(0.87717086443866,-1.93250296638388,22.9261753372377));
#23852=CARTESIAN_POINT('Ctrl Pts',(-1.14779945052178,-1.78509183570046,
22.8150422192461));
#23853=CARTESIAN_POINT('Ctrl Pts',(-2.12225853141856,-0.00389439645398614,
22.7039091012546));
#23854=CARTESIAN_POINT('Ctrl Pts',(-1.15434307307923,1.78086734770913,22.592775983263));
#23855=CARTESIAN_POINT('Ctrl Pts',(0.870072600242795,1.93570920099308,22.4816428652714));
#23856=CARTESIAN_POINT('Ctrl Pts',(2.09816358409882,0.318913804756463,22.3705097472799));
#23857=CARTESIAN_POINT('Ctrl Pts',(1.4059326728736,-1.58976405791833,22.2593766292883));
#23858=CARTESIAN_POINT('Ctrl Pts',(-0.573063157536151,-2.04342728228266,
22.1482435112968));
#23859=CARTESIAN_POINT('Ctrl Pts',(-2.02756903062303,-0.62686542938788,
22.0371103933052));
#23860=CARTESIAN_POINT('Ctrl Pts',(-1.62636392254376,1.3634283376657,21.9259772753137));
#23861=CARTESIAN_POINT('Ctrl Pts',(0.263353460506672,2.1058588260709,21.8148441573221));
#23862=CARTESIAN_POINT('Ctrl Pts',(1.9120393910123,0.920924431060889,21.7037110393305));
#23863=CARTESIAN_POINT('Ctrl Pts',(1.81075161372237,-1.10687625048956,21.592577921339));
#23864=CARTESIAN_POINT('Ctrl Pts',(0.052192689072424,-2.12162022136514,
21.4814448033474));
#23865=CARTESIAN_POINT('Ctrl Pts',(-1.75413503891566,-1.19457385949326,
21.3703116853558));
#23866=CARTESIAN_POINT('Ctrl Pts',(-1.95500933717726,0.825793516563662,
21.2591785673643));
#23867=CARTESIAN_POINT('Ctrl Pts',(-0.366582141691425,2.09036216333028,
21.1480454493727));
#23868=CARTESIAN_POINT('Ctrl Pts',(1.55735545850838,1.44174908239318,21.0369123313812));
#23869=CARTESIAN_POINT('Ctrl Pts',(2.055940045965,-0.526409505497094,20.9257792133896));
#23870=CARTESIAN_POINT('Ctrl Pts',(0.672847382732627,-2.01277739457252,
20.814646095398));
#23871=CARTESIAN_POINT('Ctrl Pts',(-1.32606168894103,-1.65697219019589,
20.7035129774065));
#23872=CARTESIAN_POINT('Ctrl Pts',(-2.11130690817558,0.215359180835817,
20.5923798594149));
#23873=CARTESIAN_POINT('Ctrl Pts',(-0.964200947587525,1.89058535234685,
20.4812467414234));
#23874=CARTESIAN_POINT('Ctrl Pts',(1.06537967613682,1.8354733981463,20.3701136234318));
#23875=CARTESIAN_POINT('Ctrl Pts',(2.11988287708905,0.100463943606212,20.2589805054403));
#23876=CARTESIAN_POINT('Ctrl Pts',(1.23418585083075,-1.72649406090975,20.1478473874487));
#23877=CARTESIAN_POINT('Ctrl Pts',(-0.781086681019479,-1.97329675718504,
20.0367142694571));
#23878=CARTESIAN_POINT('Ctrl Pts',(-2.08147786640381,-0.414060572995714,
19.9255811514656));
#23879=CARTESIAN_POINT('Ctrl Pts',(-1.47681872209176,1.52414010625231,19.814448033474));
#23880=CARTESIAN_POINT('Ctrl Pts',(0.479483312463692,2.06738784491702,19.7033149154825));
#23881=CARTESIAN_POINT('Ctrl Pts',(1.99694283049276,0.718480713622634,19.5921817974909));
#23882=CARTESIAN_POINT('Ctrl Pts',(1.68672266442399,-1.28800797157924,19.4810486794994));
#23883=CARTESIAN_POINT('Ctrl Pts',(-0.167254382363781,-2.11566159305851,
19.3699155615078));
#23884=CARTESIAN_POINT('Ctrl Pts',(-1.86814996453264,-1.0069774391256,19.2587824435162));
#23885=CARTESIAN_POINT('Ctrl Pts',(-1.85924822631064,1.0233301523674,19.1476493255247));
#23886=CARTESIAN_POINT('Ctrl Pts',(-0.148675765957402,2.11704945726364,
19.0365162075331));
#23887=CARTESIAN_POINT('Ctrl Pts',(1.69794452754165,1.27315456984867,18.9253830895415));
#23888=CARTESIAN_POINT('Ctrl Pts',(1.99058929493877,-0.735967644051852,
18.81424997155));
#23889=CARTESIAN_POINT('Ctrl Pts',(0.461272008464836,-2.07152992199117,
18.7031168535584));
#23890=CARTESIAN_POINT('Ctrl Pts',(-1.49003428616897,-1.51109530584743,
18.5919837355669));
#23891=CARTESIAN_POINT('Ctrl Pts',(-2.07795878442334,0.43225481623207,18.4808506175753));
#23892=CARTESIAN_POINT('Ctrl Pts',(-0.763368548172731,1.9801776096923,18.3697174995837));
#23893=CARTESIAN_POINT('Ctrl Pts',(1.24856735077038,1.71539873057631,18.2585843815922));
#23894=CARTESIAN_POINT('Ctrl Pts',(2.12032280000797,-0.118666593922666,
18.1474512636006));
#23895=CARTESIAN_POINT('Ctrl Pts',(1.04636073931038,-1.84560680034591,18.0363181456091));
#23896=CARTESIAN_POINT('Ctrl Pts',(-0.300314735083234,-1.86826056061615,
17.9622294002814));
#23897=CARTESIAN_POINT('Ctrl Pts',(-0.829785877867478,-1.59234886373437,
17.9251850276175));
#23898=CARTESIAN_POINT('Ctrl Pts',(-0.429864256885881,-1.60958774866484,
29.2244449171475));
#23899=CARTESIAN_POINT('Ctrl Pts',(-0.965067492876795,-1.46665379460549,
29.1874005444836));
#23900=CARTESIAN_POINT('Ctrl Pts',(-1.87243069143824,-0.607377246303806,
29.1133117991559));
#23901=CARTESIAN_POINT('Ctrl Pts',(-1.52533145026359,1.24730530523812,29.0021786811643));
#23902=CARTESIAN_POINT('Ctrl Pts',(0.220381886651061,1.95618532526583,28.8910455631728));
#23903=CARTESIAN_POINT('Ctrl Pts',(1.76309023385211,0.876778588782393,28.7799124451812));
#23904=CARTESIAN_POINT('Ctrl Pts',(1.69282300260543,-1.00616693362718,28.6687793271896));
#23905=CARTESIAN_POINT('Ctrl Pts',(0.0728673284468312,-1.96767010293874,
28.5576462091981));
#23906=CARTESIAN_POINT('Ctrl Pts',(-1.61359726760772,-1.12857467982718,
28.4465130912066));
#23907=CARTESIAN_POINT('Ctrl Pts',(-1.82332886694028,0.743587825643046,
28.335379973215));
#23908=CARTESIAN_POINT('Ctrl Pts',(-0.364228843964538,1.93511088026123,
28.2242468552234));
#23909=CARTESIAN_POINT('Ctrl Pts',(1.4282021196846,1.3555851808516,28.1131137372319));
#23910=CARTESIAN_POINT('Ctrl Pts',(1.91349962378789,-0.464646700892107,
28.0019806192403));
#23911=CARTESIAN_POINT('Ctrl Pts',(0.647480021579331,-1.85960456970283,
27.8908475012488));
#23912=CARTESIAN_POINT('Ctrl Pts',(-1.21113517297336,-1.55258489824498,
27.7797143832572));
#23913=CARTESIAN_POINT('Ctrl Pts',(-1.96127366419753,0.175424574994203,
27.6685812652656));
#23914=CARTESIAN_POINT('Ctrl Pts',(-0.916376326699777,1.74287701526117,
27.5574481472741));
#23915=CARTESIAN_POINT('Ctrl Pts',(0.967224185379086,1.71518062226255,27.4463150292825));
#23916=CARTESIAN_POINT('Ctrl Pts',(1.96558331759158,0.117682993534743,27.335181911291));
#23917=CARTESIAN_POINT('Ctrl Pts',(1.16496309552525,-1.58752252363869,27.2240487932994));
#23918=CARTESIAN_POINT('Ctrl Pts',(-0.701877132586712,-1.83976505692104,
27.1129156753079));
#23919=CARTESIAN_POINT('Ctrl Pts',(-1.92633182052286,-0.408182138351005,
27.0017825573162));
#23920=CARTESIAN_POINT('Ctrl Pts',(-1.3877317872934,1.39698510827778,26.8906494393248));
#23921=CARTESIAN_POINT('Ctrl Pts',(0.420974988196826,1.92357661506153,26.7795163213331));
#23922=CARTESIAN_POINT('Ctrl Pts',(1.8443888903088,0.689635084154899,26.6683832033416));
#23923=CARTESIAN_POINT('Ctrl Pts',(1.57974548284846,-1.1754876152001,26.55725008535));
#23924=CARTESIAN_POINT('Ctrl Pts',(-0.130743167274974,-1.96475778464122,
26.4461169673585));
#23925=CARTESIAN_POINT('Ctrl Pts',(-1.72157052544407,-0.955804296290804,
26.3349838493669));
#23926=CARTESIAN_POINT('Ctrl Pts',(-1.73674877798798,0.927938903504224,
26.2238507313754));
#23927=CARTESIAN_POINT('Ctrl Pts',(-0.16238619135084,1.9623958958108,26.1127176133838));
#23928=CARTESIAN_POINT('Ctrl Pts',(1.56059862917248,1.20079092495615,26.0015844953923));
#23929=CARTESIAN_POINT('Ctrl Pts',(1.85526215965974,-0.659825163002576,
25.8904513774007));
#23930=CARTESIAN_POINT('Ctrl Pts',(0.451916739247426,-1.91654329136076,
25.7793182594092));
#23931=CARTESIAN_POINT('Ctrl Pts',(-1.36504066820824,-1.41916556503343,
25.6681851414176));
#23932=CARTESIAN_POINT('Ctrl Pts',(-1.93265912863499,0.377088344212721,
25.557052023426));
#23933=CARTESIAN_POINT('Ctrl Pts',(-0.731431885816894,1.82821615878909,
25.4459189054345));
#23934=CARTESIAN_POINT('Ctrl Pts',(1.13923060778136,1.60608858695159,25.3347857874429));
#23935=CARTESIAN_POINT('Ctrl Pts',(1.96722440945728,-0.0859944746930651,
25.2236526694514));
#23936=CARTESIAN_POINT('Ctrl Pts',(0.994737002400207,-1.69937200838998,
25.1125195514598));
#23937=CARTESIAN_POINT('Ctrl Pts',(-0.88817286172071,-1.75741739337746,
25.0013864334682));
#23938=CARTESIAN_POINT('Ctrl Pts',(-1.9581919646515,-0.207005208671568,
24.8902533154767));
#23939=CARTESIAN_POINT('Ctrl Pts',(-1.23599670784864,1.53286629065628,24.7791201974851));
#23940=CARTESIAN_POINT('Ctrl Pts',(0.6174313843337,1.86979822774616,24.6679870794936));
#23941=CARTESIAN_POINT('Ctrl Pts',(1.90576197171134,0.495417232261691,24.556853961502));
#23942=CARTESIAN_POINT('Ctrl Pts',(1.44986419251851,-1.33238911362094,24.4457208435104));
#23943=CARTESIAN_POINT('Ctrl Pts',(-0.333006361765792,-1.9407405003932,
24.3345877255189));
#23944=CARTESIAN_POINT('Ctrl Pts',(-1.81109638675937,-0.772849794403871,
24.2234546075273));
#23945=CARTESIAN_POINT('Ctrl Pts',(-1.63159971453162,1.10238346249536,24.1123214895358));
#23946=CARTESIAN_POINT('Ctrl Pts',(0.0412012355744378,1.96867198512857,
24.0011883715442));
#23947=CARTESIAN_POINT('Ctrl Pts',(1.67629319321794,1.03315442079785,23.8900552535526));
#23948=CARTESIAN_POINT('Ctrl Pts',(1.77717564217123,-0.847946734008808,
23.7789221355611));
#23949=CARTESIAN_POINT('Ctrl Pts',(0.251516994457764,-1.95297366299238,
23.6677890175695));
#23950=CARTESIAN_POINT('Ctrl Pts',(-1.50433990619589,-1.270562227311,23.556655899578));
#23951=CARTESIAN_POINT('Ctrl Pts',(-1.88336571445733,0.574717767647355,
23.4455227815863));
#23952=CARTESIAN_POINT('Ctrl Pts',(-0.538661092295258,1.89399344098395,
23.3343896635949));
#23953=CARTESIAN_POINT('Ctrl Pts',(1.29904736302942,1.47981177027663,23.2232565456032));
#23954=CARTESIAN_POINT('Ctrl Pts',(1.94781654170361,-0.288751877411564,
23.1121234276117));
#23955=CARTESIAN_POINT('Ctrl Pts',(0.813867356098656,-1.79303844172955,
23.0009903096202));
#23956=CARTESIAN_POINT('Ctrl Pts',(-1.06496526731478,-1.65626565087129,
22.8898571916286));
#23957=CARTESIAN_POINT('Ctrl Pts',(-1.96909976145727,-0.00361334635485625,
22.778724073637));
#23958=CARTESIAN_POINT('Ctrl Pts',(-1.07103665090268,1.65234603496547,22.6675909556455));
#23959=CARTESIAN_POINT('Ctrl Pts',(0.807281358149812,1.7960132893792,22.5564578376539));
#23960=CARTESIAN_POINT('Ctrl Pts',(1.946743693939,0.295898490958891,22.4453247196624));
#23961=CARTESIAN_POINT('Ctrl Pts',(1.30446957795002,-1.47503425283813,22.3341916016708));
#23962=CARTESIAN_POINT('Ctrl Pts',(-0.531706439200944,-1.89595759165521,
22.2230584836793));
#23963=CARTESIAN_POINT('Ctrl Pts',(-1.88124379543396,-0.581625918425882,
22.1119253656877));
#23964=CARTESIAN_POINT('Ctrl Pts',(-1.50899278505104,1.26503268792002,22.0007922476961));
#23965=CARTESIAN_POINT('Ctrl Pts',(0.244347815586829,1.95388358707985,21.8896591297046));
#23966=CARTESIAN_POINT('Ctrl Pts',(1.77405167796528,0.854463323236147,21.778526011713));
#23967=CARTESIAN_POINT('Ctrl Pts',(1.68007361867256,-1.02699540538299,21.6673928937215));
#23968=CARTESIAN_POINT('Ctrl Pts',(0.0484260565246162,-1.96850751684837,
21.5562597757299));
#23969=CARTESIAN_POINT('Ctrl Pts',(-1.62754293859943,-1.10836406919707,
21.4451266577384));
#23970=CARTESIAN_POINT('Ctrl Pts',(-1.81392057682497,0.766197799375352,
21.3339935397467));
#23971=CARTESIAN_POINT('Ctrl Pts',(-0.340126707973034,1.93950528469388,
21.2228604217553));
#23972=CARTESIAN_POINT('Ctrl Pts',(1.44496451137047,1.33770119530349,21.1117273037636));
#23973=CARTESIAN_POINT('Ctrl Pts',(1.90756733647061,-0.488419679486605,
21.0005941857721));
#23974=CARTESIAN_POINT('Ctrl Pts',(0.624289454475828,-1.86751963949941,
20.8894610677805));
#23975=CARTESIAN_POINT('Ctrl Pts',(-1.2303627087441,-1.53739212077766,20.778327949789));
#23976=CARTESIAN_POINT('Ctrl Pts',(-1.95893849298029,0.19981717841322,20.6671948317974));
#23977=CARTESIAN_POINT('Ctrl Pts',(-0.894616667943091,1.75414593048305,
20.5560617138059));
#23978=CARTESIAN_POINT('Ctrl Pts',(0.988493548304972,1.70301128582823,20.4449285958143));
#23979=CARTESIAN_POINT('Ctrl Pts',(1.96689555291986,0.0932136798893295,
20.3337954778228));
#23980=CARTESIAN_POINT('Ctrl Pts',(1.14511734950612,-1.60189674969638,20.2226623598312));
#23981=CARTESIAN_POINT('Ctrl Pts',(-0.7247173586551,-1.83088823361226,20.1115292418396));
#23982=CARTESIAN_POINT('Ctrl Pts',(-1.93126214810159,-0.384178724431723,
20.0003961238481));
#23983=CARTESIAN_POINT('Ctrl Pts',(-1.37023993558539,1.41414623865022,19.8892630058565));
#23984=CARTESIAN_POINT('Ctrl Pts',(0.444880047467124,1.91818897273778,19.778129887865));
#23985=CARTESIAN_POINT('Ctrl Pts',(1.85282782137705,0.666629527393313,19.6669967698734));
#23986=CARTESIAN_POINT('Ctrl Pts',(1.56499556816097,-1.19505524517623,19.5558636518819));
#23987=CARTESIAN_POINT('Ctrl Pts',(-0.15518399833929,-1.96297890975197,
19.4447305338902));
#23988=CARTESIAN_POINT('Ctrl Pts',(-1.73332965567998,-0.934306073374439,
19.3335974158987));
#23989=CARTESIAN_POINT('Ctrl Pts',(-1.72507033649243,0.949478646963803,
19.2224642979071));
#23990=CARTESIAN_POINT('Ctrl Pts',(-0.137946160162454,1.96426661482409,
19.1113311799156));
#23991=CARTESIAN_POINT('Ctrl Pts',(1.57540757389023,1.18127378105604,19.000198061924));
#23992=CARTESIAN_POINT('Ctrl Pts',(1.8469328066281,-0.682854464189196,18.8890649439325));
#23993=CARTESIAN_POINT('Ctrl Pts',(0.427983013562401,-1.9220321251426,18.7779318259409));
#23994=CARTESIAN_POINT('Ctrl Pts',(-1.38250176122384,-1.40204285304227,
18.6667987079494));
#23995=CARTESIAN_POINT('Ctrl Pts',(-1.92799703059319,0.401059928811971,
18.5556655899578));
#23996=CARTESIAN_POINT('Ctrl Pts',(-0.708277904815949,1.83727250999993,
18.4445324719662));
#23997=CARTESIAN_POINT('Ctrl Pts',(1.15846096795848,1.59160214515625,18.3333993539747));
#23998=CARTESIAN_POINT('Ctrl Pts',(1.96730372756111,-0.110102684629042,
18.2222662359831));
#23999=CARTESIAN_POINT('Ctrl Pts',(0.97084716667254,-1.71241338249015,18.1111331179916));
#24000=CARTESIAN_POINT('Ctrl Pts',(-0.278641675582867,-1.73343227028533,
18.0370443726639));
#24001=CARTESIAN_POINT('Ctrl Pts',(-0.76990204067047,-1.47743251885541,
18.));
#24002=CARTESIAN_POINT('Ctrl Pts',(-1.6638200260918,0.000942871389988137,
28.3785196366098));
#24003=CARTESIAN_POINT('Ctrl Pts',(-1.66493926816573,0.216633787367396,
28.3641397488115));
#24004=CARTESIAN_POINT('Ctrl Pts',(-1.62602025375689,0.431937629364058,
28.3497598610133));
#24005=CARTESIAN_POINT('Ctrl Pts',(-1.54519026322223,0.630147917167703,
28.335379973215));
#24006=CARTESIAN_POINT('Ctrl Pts',(-1.33696219261504,1.14076217718244,28.2983356005511));
#24007=CARTESIAN_POINT('Ctrl Pts',(-0.850595518289787,1.53793652872184,
28.2612912278873));
#24008=CARTESIAN_POINT('Ctrl Pts',(-0.308673687185639,1.63993608792326,
28.2242468552234));
#24009=CARTESIAN_POINT('Ctrl Pts',(0.23324814391851,1.74193564712469,28.1872024825596));
#24010=CARTESIAN_POINT('Ctrl Pts',(0.830725131801557,1.54876041398814,28.1501581098957));
#24011=CARTESIAN_POINT('Ctrl Pts',(1.21034654309363,1.14880081712925,28.1131137372319));
#24012=CARTESIAN_POINT('Ctrl Pts',(1.5899679543857,0.748841220270365,28.076069364568));
#24013=CARTESIAN_POINT('Ctrl Pts',(1.75173378908679,0.142097259689129,28.0390249919042));
#24014=CARTESIAN_POINT('Ctrl Pts',(1.62161343940258,-0.393767698736607,
28.0019806192403));
#24015=CARTESIAN_POINT('Ctrl Pts',(1.49149308971837,-0.929632657162347,
27.9649362465765));
#24016=CARTESIAN_POINT('Ctrl Pts',(1.06948655564886,-1.39461861343258,27.9278918739126));
#24017=CARTESIAN_POINT('Ctrl Pts',(0.548714089521982,-1.57594164632473,
27.8908475012488));
#24018=CARTESIAN_POINT('Ctrl Pts',(0.0279416233951079,-1.75726467921688,
27.8538031285849));
#24019=CARTESIAN_POINT('Ctrl Pts',(-0.591596774789128,-1.65492478873093,
27.8167587559211));
#24020=CARTESIAN_POINT('Ctrl Pts',(-1.02638905575194,-1.31575326461476,
27.7797143832572));
#24021=CARTESIAN_POINT('Ctrl Pts',(-1.42229889353421,-1.00691304602614,
27.7459828010414));
#24022=CARTESIAN_POINT('Ctrl Pts',(-1.66502795857797,-0.501705763306371,
27.7122512188256));
#24023=CARTESIAN_POINT('Ctrl Pts',(-1.66818493320164,0.000858898907110364,
27.6785196366098));
#24024=CARTESIAN_POINT('Ctrl Pts',(-0.530170217188634,-1.98517432567172,
29.));
#24025=CARTESIAN_POINT('Ctrl Pts',(-0.598844984340848,-1.9597466054765,
29.));
#24026=CARTESIAN_POINT('Ctrl Pts',(-0.665816349367419,-1.93043078959701,
29.));
#24027=CARTESIAN_POINT('Ctrl Pts',(-0.730895187105961,-1.8975204208506,
29.));
#24028=CARTESIAN_POINT('Ctrl Pts',(-0.797776356373901,-1.86369861303587,
29.));
#24029=CARTESIAN_POINT('Ctrl Pts',(-0.862659492565893,-1.82607970767592,
29.));
#24030=CARTESIAN_POINT('Ctrl Pts',(-0.925308102267728,-1.78493769378496,
29.));
#24031=CARTESIAN_POINT('Ctrl Pts',(-0.978240206862307,-1.75017661300644,
29.));
#24032=CARTESIAN_POINT('Ctrl Pts',(-1.02957682932671,-1.71289946201033,
29.));
#24033=CARTESIAN_POINT('Ctrl Pts',(-1.07915259076278,-1.67325348841043,
29.));
#24034=CARTESIAN_POINT('Ctrl Pts',(-1.10117709167781,-1.65564038965945,
29.));
#24035=CARTESIAN_POINT('Ctrl Pts',(-1.12285375455339,-1.63755958589035,
29.));
#24036=CARTESIAN_POINT('Ctrl Pts',(-1.14416652638477,-1.61902326437413,
29.));
#24037=CARTESIAN_POINT('Ctrl Pts',(-1.15588198328982,-1.60883399956992,
29.));
#24038=CARTESIAN_POINT('Ctrl Pts',(-1.16748746879726,-1.59850708840077,
29.));
#24039=CARTESIAN_POINT('Ctrl Pts',(-1.17898018224506,-1.58804451337869,
29.));
#24040=CARTESIAN_POINT('Ctrl Pts',(-1.18957053268403,-1.57840341891643,
29.));
#24041=CARTESIAN_POINT('Ctrl Pts',(-1.20006655223653,-1.56864561876181,
29.));
#24042=CARTESIAN_POINT('Ctrl Pts',(-1.21045017554235,-1.55878810261091,
29.));
#24043=CARTESIAN_POINT('Ctrl Pts',(-1.26353644073431,-1.50839155979456,
29.));
#24044=CARTESIAN_POINT('Ctrl Pts',(-1.31378278231012,-1.45530711011964,
29.));
#24045=CARTESIAN_POINT('Ctrl Pts',(-1.36097043055599,-1.3997936077315,29.));
#24046=CARTESIAN_POINT('Ctrl Pts',(-1.40778995980368,-1.34471317576845,
29.));
#24047=CARTESIAN_POINT('Ctrl Pts',(-1.45159884056718,-1.28724056013132,
29.));
#24048=CARTESIAN_POINT('Ctrl Pts',(-1.4921385971107,-1.22760436053223,29.));
#24049=CARTESIAN_POINT('Ctrl Pts',(-1.5258287787978,-1.17804426025226,29.));
#24050=CARTESIAN_POINT('Ctrl Pts',(-1.55726056691569,-1.12698927604103,
29.));
#24051=CARTESIAN_POINT('Ctrl Pts',(-1.58625800648523,-1.07456412141552,
29.));
#24052=CARTESIAN_POINT('Ctrl Pts',(-1.59836554642316,-1.052674614521,29.));
#24053=CARTESIAN_POINT('Ctrl Pts',(-1.6100483646418,-1.03054619530609,29.));
#24054=CARTESIAN_POINT('Ctrl Pts',(-1.62129221084824,-1.00818785804745,
29.));
#24055=CARTESIAN_POINT('Ctrl Pts',(-1.62649432232627,-0.997843482933499,
29.));
#24056=CARTESIAN_POINT('Ctrl Pts',(-1.63160245634821,-0.987449892279893,
29.));
#24057=CARTESIAN_POINT('Ctrl Pts',(-1.63661513633768,-0.977007978776379,
29.));
#24058=CARTESIAN_POINT('Ctrl Pts',(-1.64184640941963,-0.96611071400989,
29.));
#24059=CARTESIAN_POINT('Ctrl Pts',(-1.64697010952128,-0.955168277699256,
29.));
#24060=CARTESIAN_POINT('Ctrl Pts',(-1.6519831845252,-0.944185960007519,
29.));
#24061=CARTESIAN_POINT('Ctrl Pts',(-1.68052299443904,-0.881662806236541,
29.));
#24062=CARTESIAN_POINT('Ctrl Pts',(-1.70550187231934,-0.817805134572764,
29.));
#24063=CARTESIAN_POINT('Ctrl Pts',(-1.72669629748412,-0.752816828589081,
29.));
#24064=CARTESIAN_POINT('Ctrl Pts',(-1.74589987179783,-0.693933053550302,
29.));
#24065=CARTESIAN_POINT('Ctrl Pts',(-1.76199624844007,-0.634120477883048,
29.));
#24066=CARTESIAN_POINT('Ctrl Pts',(-1.77478245715023,-0.573525911714975,
29.));
#24067=CARTESIAN_POINT('Ctrl Pts',(-1.78991431693715,-0.501815172441987,
29.));
#24068=CARTESIAN_POINT('Ctrl Pts',(-1.80041069773216,-0.42900768942451,
29.));
#24069=CARTESIAN_POINT('Ctrl Pts',(-1.80634685634798,-0.355527190631044,
29.));
#24070=CARTESIAN_POINT('Ctrl Pts',(-1.80765324390704,-0.339356125187838,
29.));
#24071=CARTESIAN_POINT('Ctrl Pts',(-1.80873854664514,-0.323152545934638,
29.));
#24072=CARTESIAN_POINT('Ctrl Pts',(-1.80960319748954,-0.306921133556182,
29.));
#24073=CARTESIAN_POINT('Ctrl Pts',(-1.81049819138598,-0.290120114852003,
29.));
#24074=CARTESIAN_POINT('Ctrl Pts',(-1.81115678487511,-0.27328307874498,
29.));
#24075=CARTESIAN_POINT('Ctrl Pts',(-1.81157889796795,-0.256449498362707,
29.));
#24076=CARTESIAN_POINT('Ctrl Pts',(-1.81329830981387,-0.18788053424027,
29.));
#24077=CARTESIAN_POINT('Ctrl Pts',(-1.81110575709439,-0.119282211213726,
29.));
#24078=CARTESIAN_POINT('Ctrl Pts',(-1.80512192796928,-0.0509934048330952,
29.));
#24079=CARTESIAN_POINT('Ctrl Pts',(-1.79913941487413,0.0172803827172064,
29.));
#24080=CARTESIAN_POINT('Ctrl Pts',(-1.78936683881028,0.0852458626519091,
29.));
#24081=CARTESIAN_POINT('Ctrl Pts',(-1.77587520290159,0.152549360262613,
29.));
#24082=CARTESIAN_POINT('Ctrl Pts',(-1.76611529025284,0.2012370258712,29.));
#24083=CARTESIAN_POINT('Ctrl Pts',(-1.75440809028966,0.249578001150906,
29.));
#24084=CARTESIAN_POINT('Ctrl Pts',(-1.74076629009681,0.297428750832602,
29.));
#24085=CARTESIAN_POINT('Ctrl Pts',(-1.73053117355718,0.333330024313932,
29.));
#24086=CARTESIAN_POINT('Ctrl Pts',(-1.71920679407154,0.368955188045359,
29.));
#24087=CARTESIAN_POINT('Ctrl Pts',(-1.70679459856354,0.404239446148925,
29.));
#24088=CARTESIAN_POINT('Ctrl Pts',(-1.70266053149517,0.415991395218995,
29.));
#24089=CARTESIAN_POINT('Ctrl Pts',(-1.69840897216887,0.427696366036902,
29.));
#24090=CARTESIAN_POINT('Ctrl Pts',(-1.69404059684701,0.439351704919061,
29.));
#24091=CARTESIAN_POINT('Ctrl Pts',(-1.67091592294313,0.501051053310776,
29.));
#24092=CARTESIAN_POINT('Ctrl Pts',(-1.64451911211263,0.561366930679729,
29.));
#24093=CARTESIAN_POINT('Ctrl Pts',(-1.61490024705089,0.619964816031714,
29.));
#24094=CARTESIAN_POINT('Ctrl Pts',(-1.5940694639762,0.661176382911764,29.));
#24095=CARTESIAN_POINT('Ctrl Pts',(-1.57164412390922,0.701537662145848,
29.));
#24096=CARTESIAN_POINT('Ctrl Pts',(-1.5476312537223,0.740920937772863,29.));
#24097=CARTESIAN_POINT('Ctrl Pts',(-1.53991733315498,0.75357246412114,29.));
#24098=CARTESIAN_POINT('Ctrl Pts',(-1.53203843675107,0.766124659274376,
29.));
#24099=CARTESIAN_POINT('Ctrl Pts',(-1.52399809481428,0.778567695014452,
29.));
#24100=CARTESIAN_POINT('Ctrl Pts',(-1.48975623557589,0.831559555517324,
29.));
#24101=CARTESIAN_POINT('Ctrl Pts',(-1.45265940234734,0.882467052899552,
29.));
#24102=CARTESIAN_POINT('Ctrl Pts',(-1.4127419174334,0.930974609595389,29.));
#24103=CARTESIAN_POINT('Ctrl Pts',(-1.37594260255018,0.975692979425408,
29.));
#24104=CARTESIAN_POINT('Ctrl Pts',(-1.33674551146281,1.0183718057298,29.));
#24105=CARTESIAN_POINT('Ctrl Pts',(-1.29515607471415,1.05873088388067,29.));
#24106=CARTESIAN_POINT('Ctrl Pts',(-1.28733756798151,1.06631809229016,29.));
#24107=CARTESIAN_POINT('Ctrl Pts',(-1.27943445976865,1.07382321453206,29.));
#24108=CARTESIAN_POINT('Ctrl Pts',(-1.27144834193523,1.08124558643406,29.));
#24109=CARTESIAN_POINT('Origin',(0.,0.,23.));
#24110=CARTESIAN_POINT('Origin',(0.,0.,17.));
#24111=CARTESIAN_POINT('Origin',(6.,-1.,-2.));
#24112=CARTESIAN_POINT('',(-6.,-1.,-2.));
#24113=CARTESIAN_POINT('',(6.,-1.,-2.));
#24114=CARTESIAN_POINT('',(-6.,-1.,-2.));
#24115=CARTESIAN_POINT('',(6.,-1.,-5.));
#24116=CARTESIAN_POINT('',(6.,-1.,-2.));
#24117=CARTESIAN_POINT('',(-6.,-1.,-5.));
#24118=CARTESIAN_POINT('',(3.,-1.,-5.));
#24119=CARTESIAN_POINT('',(-6.,-1.,-2.));
#24120=CARTESIAN_POINT('Origin',(6.,1.,-2.));
#24121=CARTESIAN_POINT('',(6.,1.,-2.));
#24122=CARTESIAN_POINT('',(6.,-1.,-2.));
#24123=CARTESIAN_POINT('',(6.,1.,-5.));
#24124=CARTESIAN_POINT('',(6.,1.,-2.));
#24125=CARTESIAN_POINT('',(6.,0.5,-5.));
#24126=CARTESIAN_POINT('Origin',(-6.,1.,-2.));
#24127=CARTESIAN_POINT('',(-6.,1.,-2.));
#24128=CARTESIAN_POINT('',(6.,1.,-2.));
#24129=CARTESIAN_POINT('',(-6.,1.,-5.));
#24130=CARTESIAN_POINT('',(-6.,1.,-2.));
#24131=CARTESIAN_POINT('',(-3.,1.,-5.));
#24132=CARTESIAN_POINT('Origin',(-6.,-1.,-2.));
#24133=CARTESIAN_POINT('',(-6.,1.,-2.));
#24134=CARTESIAN_POINT('',(-6.,-0.5,-5.));
#24135=CARTESIAN_POINT('Origin',(0.,0.,-2.));
#24136=CARTESIAN_POINT('Origin',(0.,0.,4.));
#24137=CARTESIAN_POINT('',(-3.,-3.67394039744206E-16,3.));
#24138=CARTESIAN_POINT('Origin',(0.,0.,3.));
#24139=CARTESIAN_POINT('',(-3.,-3.67394039744206E-16,5.));
#24140=CARTESIAN_POINT('',(-3.,-3.67394039744206E-16,4.));
#24141=CARTESIAN_POINT('Origin',(0.,0.,5.));
#24142=CARTESIAN_POINT('Origin',(7.,0.,3.));
#24143=CARTESIAN_POINT('',(-4.,4.89858719658941E-16,3.));
#24144=CARTESIAN_POINT('Origin',(0.,0.,3.));
#24145=CARTESIAN_POINT('Origin',(3.,0.,5.));
#24146=CARTESIAN_POINT('',(-4.,-4.89858719658941E-16,5.));
#24147=CARTESIAN_POINT('Origin',(0.,0.,5.));
#24148=CARTESIAN_POINT('Origin',(0.,0.,0.));
#24149=CARTESIAN_POINT('',(-4.,-4.89858719658941E-16,25.));
#24150=CARTESIAN_POINT('Origin',(0.,0.,25.));
#24151=CARTESIAN_POINT('',(-4.,-4.89858719658941E-16,0.));
#24152=CARTESIAN_POINT('Origin',(-1.73205080756888,-3.,25.));
#24153=CARTESIAN_POINT('',(1.73205080756888,-3.,25.));
#24154=CARTESIAN_POINT('',(-1.73205080756888,-3.,25.));
#24155=CARTESIAN_POINT('',(-0.86602540378444,-3.,25.));
#24156=CARTESIAN_POINT('',(1.73205080756888,-3.,29.));
#24157=CARTESIAN_POINT('',(1.73205080756888,-3.,25.));
#24158=CARTESIAN_POINT('',(-1.73205080756888,-3.,29.));
#24159=CARTESIAN_POINT('',(-1.73205080756888,-3.,29.));
#24160=CARTESIAN_POINT('',(-1.73205080756888,-3.,25.));
#24161=CARTESIAN_POINT('Origin',(-3.46410161513775,4.24230095489963E-16,
25.));
#24162=CARTESIAN_POINT('',(-3.46410161513775,4.24230095489963E-16,25.));
#24163=CARTESIAN_POINT('',(-3.03108891324554,-0.749999999999999,25.));
#24164=CARTESIAN_POINT('',(-3.46410161513775,5.55111512312578E-16,29.));
#24165=CARTESIAN_POINT('',(-3.46410161513775,4.24230095489963E-16,29.));
#24166=CARTESIAN_POINT('',(-3.46410161513775,4.24230095489963E-16,25.));
#24167=CARTESIAN_POINT('Origin',(-1.73205080756888,3.,25.));
#24168=CARTESIAN_POINT('',(-1.73205080756888,3.,25.));
#24169=CARTESIAN_POINT('',(-2.1650635094611,2.25,25.));
#24170=CARTESIAN_POINT('',(-1.73205080756888,3.,29.));
#24171=CARTESIAN_POINT('',(-1.73205080756888,3.,29.));
#24172=CARTESIAN_POINT('',(-1.73205080756888,3.,25.));
#24173=CARTESIAN_POINT('Origin',(1.73205080756888,3.,25.));
#24174=CARTESIAN_POINT('',(1.73205080756888,3.,25.));
#24175=CARTESIAN_POINT('',(0.866025403784439,3.,25.));
#24176=CARTESIAN_POINT('',(1.73205080756888,3.,29.));
#24177=CARTESIAN_POINT('',(1.73205080756888,3.,29.));
#24178=CARTESIAN_POINT('',(1.73205080756888,3.,25.));
#24179=CARTESIAN_POINT('Origin',(3.46410161513775,0.,25.));
#24180=CARTESIAN_POINT('',(3.46410161513775,0.,25.));
#24181=CARTESIAN_POINT('',(3.03108891324554,0.75,25.));
#24182=CARTESIAN_POINT('',(3.46410161513775,0.,29.));
#24183=CARTESIAN_POINT('',(3.46410161513775,0.,29.));
#24184=CARTESIAN_POINT('',(3.46410161513775,0.,25.));
#24185=CARTESIAN_POINT('Origin',(1.73205080756888,-3.,25.));
#24186=CARTESIAN_POINT('',(2.1650635094611,-2.25,25.));
#24187=CARTESIAN_POINT('',(1.73205080756888,-3.,29.));
#24188=CARTESIAN_POINT('Origin',(0.,5.55111512312578E-16,29.));
#24189=CARTESIAN_POINT('Origin',(0.,0.,0.));
#24190=CARTESIAN_POINT('',(-10.,-1.22464679914735E-15,0.));
#24191=CARTESIAN_POINT('Origin',(0.,0.,0.));
#24192=CARTESIAN_POINT('',(-4.,-4.89858719658941E-16,0.));
#24193=CARTESIAN_POINT('Origin',(0.,0.,0.));
#24194=CARTESIAN_POINT('Origin',(0.,0.,-5.));
#24195=CARTESIAN_POINT('',(-10.,-1.22464679914735E-15,-5.));
#24196=CARTESIAN_POINT('',(-10.,-1.22464679914735E-15,-5.));
#24197=CARTESIAN_POINT('Origin',(0.,0.,-5.));
#24198=CARTESIAN_POINT('Origin',(0.,0.,-5.));
#24199=CARTESIAN_POINT('Origin',(0.,0.,0.));
#24200=CARTESIAN_POINT('',(-4.,-4.89858719658941E-16,0.));
#24201=CARTESIAN_POINT('Origin',(0.,0.,25.));
#24202=CARTESIAN_POINT('',(0.,0.,0.));
#24203=CARTESIAN_POINT('Origin',(1.73205080756888,3.,4.));
#24204=CARTESIAN_POINT('',(1.73205080756888,3.,4.));
#24205=CARTESIAN_POINT('',(3.46410161513775,0.,4.));
#24206=CARTESIAN_POINT('',(3.6650635094611,-0.348076211353315,4.));
#24207=CARTESIAN_POINT('',(1.73205080756888,3.,0.));
#24208=CARTESIAN_POINT('',(1.73205080756888,3.,4.));
#24209=CARTESIAN_POINT('',(3.46410161513775,0.,0.));
#24210=CARTESIAN_POINT('',(3.6650635094611,-0.348076211353316,0.));
#24211=CARTESIAN_POINT('',(3.46410161513775,0.,4.));
#24212=CARTESIAN_POINT('Origin',(-1.73205080756888,3.,4.));
#24213=CARTESIAN_POINT('',(-1.73205080756888,3.,4.));
#24214=CARTESIAN_POINT('',(5.13397459621556,3.,4.));
#24215=CARTESIAN_POINT('',(-1.73205080756888,3.,0.));
#24216=CARTESIAN_POINT('',(-1.73205080756888,3.,4.));
#24217=CARTESIAN_POINT('',(5.13397459621556,3.,0.));
#24218=CARTESIAN_POINT('Origin',(-3.46410161513775,5.55111512312578E-16,
4.));
#24219=CARTESIAN_POINT('',(-3.46410161513775,4.24230095489963E-16,4.));
#24220=CARTESIAN_POINT('',(-1.53108891324553,3.34807621135332,4.));
#24221=CARTESIAN_POINT('',(-3.46410161513775,5.55111512312578E-16,0.));
#24222=CARTESIAN_POINT('',(-3.46410161513775,4.24230095489963E-16,4.));
#24223=CARTESIAN_POINT('',(-1.53108891324553,3.34807621135332,-2.77555756156289E-16));
#24224=CARTESIAN_POINT('Origin',(-1.73205080756888,-3.,4.));
#24225=CARTESIAN_POINT('',(-1.73205080756888,-3.,4.));
#24226=CARTESIAN_POINT('',(-0.665063509461101,-4.84807621135331,4.));
#24227=CARTESIAN_POINT('',(-1.73205080756888,-3.,0.));
#24228=CARTESIAN_POINT('',(-1.73205080756888,-3.,4.));
#24229=CARTESIAN_POINT('',(-0.665063509461101,-4.84807621135332,-2.77555756156289E-16));
#24230=CARTESIAN_POINT('Origin',(1.73205080756888,-3.,4.));
#24231=CARTESIAN_POINT('',(1.73205080756888,-3.,4.));
#24232=CARTESIAN_POINT('',(6.86602540378444,-3.,4.));
#24233=CARTESIAN_POINT('',(1.73205080756888,-3.,0.));
#24234=CARTESIAN_POINT('',(1.73205080756888,-3.,4.));
#24235=CARTESIAN_POINT('',(6.86602540378444,-3.,0.));
#24236=CARTESIAN_POINT('Origin',(3.46410161513775,0.,4.));
#24237=CARTESIAN_POINT('',(4.53108891324554,1.84807621135332,4.));
#24238=CARTESIAN_POINT('',(4.53108891324553,1.84807621135332,0.));
#24239=CARTESIAN_POINT('Origin',(32.,5.,0.));
#24240=CARTESIAN_POINT('',(32.,5.,0.));
#24241=CARTESIAN_POINT('',(-8.,5.,0.));
#24242=CARTESIAN_POINT('',(32.,5.,0.));
#24243=CARTESIAN_POINT('',(-8.,5.,4.));
#24244=CARTESIAN_POINT('',(-8.,5.,0.));
#24245=CARTESIAN_POINT('',(32.,5.,4.));
#24246=CARTESIAN_POINT('',(32.,5.,4.));
#24247=CARTESIAN_POINT('',(32.,5.,0.));
#24248=CARTESIAN_POINT('Origin',(32.,-5.,0.));
#24249=CARTESIAN_POINT('',(32.,-5.,0.));
#24250=CARTESIAN_POINT('',(32.,-5.,0.));
#24251=CARTESIAN_POINT('',(32.,-5.,4.));
#24252=CARTESIAN_POINT('',(32.,-5.,4.));
#24253=CARTESIAN_POINT('',(32.,-5.,0.));
#24254=CARTESIAN_POINT('Origin',(-8.,-5.,0.));
#24255=CARTESIAN_POINT('',(-8.,-5.,0.));
#24256=CARTESIAN_POINT('',(-8.,-5.,0.));
#24257=CARTESIAN_POINT('',(-8.,-5.,4.));
#24258=CARTESIAN_POINT('',(-8.,-5.,4.));
#24259=CARTESIAN_POINT('',(-8.,-5.,0.));
#24260=CARTESIAN_POINT('Origin',(-8.,5.,0.));
#24261=CARTESIAN_POINT('',(-8.,5.,0.));
#24262=CARTESIAN_POINT('',(-8.,5.,4.));
#24263=CARTESIAN_POINT('Origin',(12.,0.,4.));
#24264=CARTESIAN_POINT('Origin',(12.,0.,0.));
#24265=CARTESIAN_POINT('',(0.,0.,0.));
#24266=CARTESIAN_POINT('Origin',(0.,0.,0.));
#24267=CARTESIAN_POINT('',(-4.,-4.89858719658941E-16,1.));
#24268=CARTESIAN_POINT('Origin',(0.,0.,1.));
#24269=CARTESIAN_POINT('',(-4.,-4.89858719658941E-16,0.));
#24270=CARTESIAN_POINT('',(-4.,-4.89858719658941E-16,0.));
#24271=CARTESIAN_POINT('Origin',(0.,0.,0.));
#24272=CARTESIAN_POINT('Origin',(0.,0.,0.));
#24273=CARTESIAN_POINT('',(-8.,-9.79717439317883E-16,1.));
#24274=CARTESIAN_POINT('Origin',(0.,0.,1.));
#24275=CARTESIAN_POINT('',(-8.,-9.79717439317883E-16,0.));
#24276=CARTESIAN_POINT('',(-8.,-9.79717439317883E-16,0.));
#24277=CARTESIAN_POINT('Origin',(0.,0.,0.));
#24278=CARTESIAN_POINT('Origin',(0.,0.,1.));
#24279=CARTESIAN_POINT('Origin',(0.,0.,0.));
#24280=CARTESIAN_POINT('',(0.,0.,0.));
#24281=CARTESIAN_POINT('Origin',(-1.,0.,1.));
#24282=CARTESIAN_POINT('',(-1.,2.82842712474619,0.));
#24283=CARTESIAN_POINT('',(-1.,2.82842712474619,1.));
#24284=CARTESIAN_POINT('',(-1.,2.82842712474619,0.));
#24285=CARTESIAN_POINT('',(-1.,5.91607978309962,0.));
#24286=CARTESIAN_POINT('',(-1.,0.,0.));
#24287=CARTESIAN_POINT('',(-1.,5.91607978309962,1.));
#24288=CARTESIAN_POINT('',(-1.,5.91607978309962,0.));
#24289=CARTESIAN_POINT('',(-1.,0.,1.));
#24290=CARTESIAN_POINT('Origin',(1.,12.,1.));
#24291=CARTESIAN_POINT('',(1.,2.82842712474619,1.));
#24292=CARTESIAN_POINT('',(1.,2.82842712474619,0.));
#24293=CARTESIAN_POINT('',(1.,2.82842712474619,0.));
#24294=CARTESIAN_POINT('',(1.,5.91607978309962,1.));
#24295=CARTESIAN_POINT('',(1.,6.,1.));
#24296=CARTESIAN_POINT('',(1.,5.91607978309962,0.));
#24297=CARTESIAN_POINT('',(1.,5.91607978309962,0.));
#24298=CARTESIAN_POINT('',(1.,6.,0.));
#24299=CARTESIAN_POINT('Origin',(0.,0.,0.));
#24300=CARTESIAN_POINT('Origin',(0.,0.,0.));
#24301=CARTESIAN_POINT('Origin',(0.,0.,0.));
#24302=CARTESIAN_POINT('Origin',(0.,0.,0.));
#24303=CARTESIAN_POINT('Origin',(0.,0.,1.));
#24304=CARTESIAN_POINT('Origin',(0.,0.,0.));
#24305=CARTESIAN_POINT('Origin',(0.,0.,1.));
#24306=CARTESIAN_POINT('Origin',(0.,0.,1.));
#24307=CARTESIAN_POINT('',(0.,0.,0.));
#24308=CARTESIAN_POINT('Origin',(0.,0.,0.));
#24309=CARTESIAN_POINT('',(-2.5,-3.06161699786838E-16,1.));
#24310=CARTESIAN_POINT('Origin',(0.,0.,1.));
#24311=CARTESIAN_POINT('',(-2.5,-3.06161699786838E-16,0.));
#24312=CARTESIAN_POINT('',(-2.5,-3.06161699786838E-16,0.));
#24313=CARTESIAN_POINT('Origin',(0.,0.,0.));
#24314=CARTESIAN_POINT('Origin',(0.,0.,0.));
#24315=CARTESIAN_POINT('',(-4.5,-5.51091059616309E-16,1.));
#24316=CARTESIAN_POINT('Origin',(0.,0.,1.));
#24317=CARTESIAN_POINT('',(-4.5,-5.51091059616309E-16,0.));
#24318=CARTESIAN_POINT('',(-4.5,-5.51091059616309E-16,0.));
#24319=CARTESIAN_POINT('Origin',(0.,0.,0.));
#24320=CARTESIAN_POINT('Origin',(0.,0.,1.));
#24321=CARTESIAN_POINT('Origin',(0.,0.,0.));
#24322=CARTESIAN_POINT('',(0.,0.,0.));
#24323=CARTESIAN_POINT('Origin',(0.,0.,0.));
#24324=CARTESIAN_POINT('',(-1.95633598837559,0.00127248296362327,0.22586969212423));
#24325=CARTESIAN_POINT('',(-1.95588590413641,0.00206796222160181,0.124130307875766));
#24326=CARTESIAN_POINT('',(-1.954,-2.39295984553393E-16,0.));
#24327=CARTESIAN_POINT('',(0.861525859670522,1.75382131162755,0.));
#24328=CARTESIAN_POINT('Ctrl Pts',(-1.95633598837559,0.00127248296362327,
0.22586969212423));
#24329=CARTESIAN_POINT('Ctrl Pts',(-1.95680065536751,0.06824838727295,0.222037687723474));
#24330=CARTESIAN_POINT('Ctrl Pts',(-1.95366001618977,0.135177367276064,
0.218205683322718));
#24331=CARTESIAN_POINT('Ctrl Pts',(-1.9467704464542,0.201714622162032,0.214373678921962));
#24332=CARTESIAN_POINT('Ctrl Pts',(-1.88018097341933,0.844814396182631,
0.177336365489126));
#24333=CARTESIAN_POINT('Ctrl Pts',(-1.46337681650964,1.45132029737704,0.140299052056291));
#24334=CARTESIAN_POINT('Ctrl Pts',(-0.886898775458456,1.74452597744752,
0.103261738623455));
#24335=CARTESIAN_POINT('Ctrl Pts',(-0.351149650411554,2.01701629862282,
0.0688411590823035));
#24336=CARTESIAN_POINT('Ctrl Pts',(0.32250805655704,2.01891265608728,0.0344205795411517));
#24337=CARTESIAN_POINT('Ctrl Pts',(0.863568564283469,1.75641400930303,6.50521303491303E-18));
#24338=CARTESIAN_POINT('',(-0.861525859670545,1.75382131162753,0.));
#24339=CARTESIAN_POINT('Origin',(0.,0.,0.));
#24340=CARTESIAN_POINT('Ctrl Pts',(-0.861525859670546,1.75382131162753,
1.07552855510562E-15));
#24341=CARTESIAN_POINT('Ctrl Pts',(-1.44517400349648,1.46711709294739,0.0370752371124262));
#24342=CARTESIAN_POINT('Ctrl Pts',(-1.86938639577653,0.868642989156275,
0.0741504742248514));
#24343=CARTESIAN_POINT('Ctrl Pts',(-1.94388330047271,0.2267475072264,0.111225711337276));
#24344=CARTESIAN_POINT('Ctrl Pts',(-1.95252655828524,0.15227369973538,0.115527243516773));
#24345=CARTESIAN_POINT('Ctrl Pts',(-1.95646228341413,0.0772153955205521,
0.119828775696269));
#24346=CARTESIAN_POINT('Ctrl Pts',(-1.95588590413641,0.00206796222160181,
0.124130307875766));
#24347=CARTESIAN_POINT('Origin',(0.,0.,0.));
#24348=CARTESIAN_POINT('',(-1.95128265771456,0.000979968443958618,0.92586969212423));
#24349=CARTESIAN_POINT('',(-1.95120671878141,0.0009421225145049,0.824130307875766));
#24350=CARTESIAN_POINT('',(-1.954,-2.39295984553393E-16,0.));
#24351=CARTESIAN_POINT('Ctrl Pts',(-1.95128265771456,0.000979968443958618,
0.92586969212423));
#24352=CARTESIAN_POINT('Ctrl Pts',(-1.95247392016078,0.26388492489574,0.910928234987155));
#24353=CARTESIAN_POINT('Ctrl Pts',(-1.90305890226364,0.526360198569273,
0.895986777850081));
#24354=CARTESIAN_POINT('Ctrl Pts',(-1.80091082202569,0.76639335768976,0.881045320713007));
#24355=CARTESIAN_POINT('Ctrl Pts',(-1.54770322455863,1.36139445209842,0.844008007280172));
#24356=CARTESIAN_POINT('Ctrl Pts',(-0.970472477077253,1.8184979102298,0.806970693847336));
#24357=CARTESIAN_POINT('Ctrl Pts',(-0.333275819998743,1.92861264524847,
0.7699333804145));
#24358=CARTESIAN_POINT('Ctrl Pts',(0.303920837079767,2.03872738026714,0.732896066981664));
#24359=CARTESIAN_POINT('Ctrl Pts',(1.00108340375541,1.8018533921731,0.695858753548828));
#24360=CARTESIAN_POINT('Ctrl Pts',(1.43928269883041,1.32632160988724,0.658821440115992));
#24361=CARTESIAN_POINT('Ctrl Pts',(1.87748199390539,0.850789827601394,0.621784126683156));
#24362=CARTESIAN_POINT('Ctrl Pts',(2.05671801737973,0.13660025112374,0.584746813250321));
#24363=CARTESIAN_POINT('Ctrl Pts',(1.89500736899678,-0.489477875405323,
0.547709499817485));
#24364=CARTESIAN_POINT('Ctrl Pts',(1.73329672061383,-1.11555600193439,0.510672186384649));
#24365=CARTESIAN_POINT('Ctrl Pts',(1.23063940037359,-1.65352267851487,0.473634872951813));
#24366=CARTESIAN_POINT('Ctrl Pts',(0.616962143929708,-1.85738653188124,
0.436597559518977));
#24367=CARTESIAN_POINT('Ctrl Pts',(0.00328488748583246,-2.06125038524761,
0.399560246086142));
#24368=CARTESIAN_POINT('Ctrl Pts',(-0.721412305161677,-1.93101141539988,
0.362522932653306));
#24369=CARTESIAN_POINT('Ctrl Pts',(-1.2255735069054,-1.52604510705262,0.32548561922047));
#24370=CARTESIAN_POINT('Ctrl Pts',(-1.67757250343746,-1.1629779682701,0.29228031018839));
#24371=CARTESIAN_POINT('Ctrl Pts',(-1.95230952873461,-0.579091046852653,
0.25907500115631));
#24372=CARTESIAN_POINT('Ctrl Pts',(-1.95633598837559,0.00127248296362327,
0.22586969212423));
#24373=CARTESIAN_POINT('Ctrl Pts',(-1.95588590413641,0.00206796222160181,
0.124130307875766));
#24374=CARTESIAN_POINT('Ctrl Pts',(-1.95149442603296,-0.570486119123227,
0.156904012808695));
#24375=CARTESIAN_POINT('Ctrl Pts',(-1.68517377795595,-1.14821417361252,
0.189677717741624));
#24376=CARTESIAN_POINT('Ctrl Pts',(-1.24335992644724,-1.51202006337354,
0.222451422674553));
#24377=CARTESIAN_POINT('Ctrl Pts',(-0.74355823061328,-1.92357529197494,
0.259526659786979));
#24378=CARTESIAN_POINT('Ctrl Pts',(-0.0191734218330693,-2.06136888910912,
0.296601896899404));
#24379=CARTESIAN_POINT('Ctrl Pts',(0.59730918482247,-1.86366268614966,0.33367713401183));
#24380=CARTESIAN_POINT('Ctrl Pts',(1.21379179147801,-1.6659564831902,0.370752371124255));
#24381=CARTESIAN_POINT('Ctrl Pts',(1.72237219600888,-1.13275048013712,0.40782760823668));
#24382=CARTESIAN_POINT('Ctrl Pts',(1.89021021423941,-0.507705222320547,
0.444902845349105));
#24383=CARTESIAN_POINT('Ctrl Pts',(2.05804823246995,0.117340035496022,0.481978082461531));
#24384=CARTESIAN_POINT('Ctrl Pts',(1.88514386440015,0.834224548076076,0.519053319573957));
#24385=CARTESIAN_POINT('Ctrl Pts',(1.45061079828058,1.31401352267999,0.556128556686382));
#24386=CARTESIAN_POINT('Ctrl Pts',(1.01607773216101,1.7938024972839,0.593203793798808));
#24387=CARTESIAN_POINT('Ctrl Pts',(0.319915967991662,2.03649593391168,0.630279030911233));
#24388=CARTESIAN_POINT('Ctrl Pts',(-0.318741968595543,1.93105881108975,
0.667354268023658));
#24389=CARTESIAN_POINT('Ctrl Pts',(-0.95739990518275,1.82562168826782,0.704429505136084));
#24390=CARTESIAN_POINT('Ctrl Pts',(-1.53855401418781,1.37205400599619,0.74150474224851));
#24391=CARTESIAN_POINT('Ctrl Pts',(-1.79588703923712,0.778131328327298,
0.778579979360935));
#24392=CARTESIAN_POINT('Ctrl Pts',(-1.9012727786294,0.534901837996683,0.793763422199212));
#24393=CARTESIAN_POINT('Ctrl Pts',(-1.95234877280959,0.268132669686638,
0.808946865037489));
#24394=CARTESIAN_POINT('Ctrl Pts',(-1.95120671878141,0.000942122514504899,
0.824130307875766));
#24395=CARTESIAN_POINT('Origin',(0.,0.,0.));
#24396=CARTESIAN_POINT('',(-1.95279514498571,-0.00168107824419284,1.62586969212423));
#24397=CARTESIAN_POINT('',(-1.95278388634516,-0.00168888116712579,1.52413030787576));
#24398=CARTESIAN_POINT('',(-1.954,-2.39295984553393E-16,0.));
#24399=CARTESIAN_POINT('Ctrl Pts',(-1.95279514498571,-0.00168107824419284,
1.62586969212423));
#24400=CARTESIAN_POINT('Ctrl Pts',(-1.94903681723145,0.45580829851081,1.59981878225084));
#24401=CARTESIAN_POINT('Ctrl Pts',(-1.78858836662353,0.915672122197071,
1.57376787237745));
#24402=CARTESIAN_POINT('Ctrl Pts',(-1.49506049969948,1.26310357403151,1.54771696250405));
#24403=CARTESIAN_POINT('Ctrl Pts',(-1.07774365121422,1.75705666974124,1.51067964907122));
#24404=CARTESIAN_POINT('Ctrl Pts',(-0.391431901374392,2.02374896425016,
1.47364233563838));
#24405=CARTESIAN_POINT('Ctrl Pts',(0.249914641927464,1.94117972705521,1.43660502220554));
#24406=CARTESIAN_POINT('Ctrl Pts',(0.891261185229321,1.85861048986026,1.39956770877271));
#24407=CARTESIAN_POINT('Ctrl Pts',(1.48764252199321,1.42677972096142,1.36253039533987));
#24408=CARTESIAN_POINT('Ctrl Pts',(1.76623794405498,0.843232102738223,1.32549308190704));
#24409=CARTESIAN_POINT('Ctrl Pts',(2.04483336611675,0.25968448451502,1.2884557684742));
#24410=CARTESIAN_POINT('Ctrl Pts',(2.0056428734764,-0.475579983032552,1.25141845504136));
#24411=CARTESIAN_POINT('Ctrl Pts',(1.66659475578394,-1.02620605156362,1.21438114160853));
#24412=CARTESIAN_POINT('Ctrl Pts',(1.32754663809148,-1.57683212009468,1.17734382817569));
#24413=CARTESIAN_POINT('Ctrl Pts',(0.688640895346918,-1.94281978960923,
1.14030651474286));
#24414=CARTESIAN_POINT('Ctrl Pts',(0.0421509461412053,-1.956746580861,1.10326920131002));
#24415=CARTESIAN_POINT('Ctrl Pts',(-0.604339003064511,-1.97067337211277,
1.06623188787719));
#24416=CARTESIAN_POINT('Ctrl Pts',(-1.25841315873137,-1.63253928510176,
1.02919457444435));
#24417=CARTESIAN_POINT('Ctrl Pts',(-1.62085801283843,-1.09702287625329,
0.992157261011514));
#24418=CARTESIAN_POINT('Ctrl Pts',(-1.83708669330173,-0.777542532858632,
0.970061404715753));
#24419=CARTESIAN_POINT('Ctrl Pts',(-1.94952098456712,-0.38781143817112,
0.947965548419991));
#24420=CARTESIAN_POINT('Ctrl Pts',(-1.95128265771456,0.000979968443958618,
0.92586969212423));
#24421=CARTESIAN_POINT('Ctrl Pts',(-1.95120671878141,0.000942122514504899,
0.824130307875766));
#24422=CARTESIAN_POINT('Ctrl Pts',(-1.94956008223784,-0.384298600093132,
0.846022102149914));
#24423=CARTESIAN_POINT('Ctrl Pts',(-1.83936019485534,-0.770415304222176,
0.867913896424062));
#24424=CARTESIAN_POINT('Ctrl Pts',(-1.62687654459384,-1.08811501975669,
0.889805690698211));
#24425=CARTESIAN_POINT('Ctrl Pts',(-1.26702108380771,-1.62616101710563,
0.926880927810636));
#24426=CARTESIAN_POINT('Ctrl Pts',(-0.613798221141896,-1.96797533873735,
0.963956164923062));
#24427=CARTESIAN_POINT('Ctrl Pts',(0.0333981997247413,-1.95692658607738,
1.00103140203549));
#24428=CARTESIAN_POINT('Ctrl Pts',(0.680594620591375,-1.94587783341741,
1.03810663914791));
#24429=CARTESIAN_POINT('Ctrl Pts',(1.32176459965883,-1.58196600646575,1.07518187626034));
#24430=CARTESIAN_POINT('Ctrl Pts',(1.66305355512094,-1.03196363523784,1.11225711337276));
#24431=CARTESIAN_POINT('Ctrl Pts',(2.00434251058304,-0.481961264009935,
1.14933235048519));
#24432=CARTESIAN_POINT('Ctrl Pts',(2.04575044243979,0.254131651494222,1.18640758759761));
#24433=CARTESIAN_POINT('Ctrl Pts',(1.76829659796069,0.838942597907999,1.22348282471004));
#24434=CARTESIAN_POINT('Ctrl Pts',(1.49084275348159,1.42375354432178,1.26055806182247));
#24435=CARTESIAN_POINT('Ctrl Pts',(0.894527132666635,1.85728252164517,1.29763329893489));
#24436=CARTESIAN_POINT('Ctrl Pts',(0.252653428905354,1.94083943808002,1.33470853604732));
#24437=CARTESIAN_POINT('Ctrl Pts',(-0.389220274855925,2.02439635451486,
1.37178377315974));
#24438=CARTESIAN_POINT('Ctrl Pts',(-1.07665206156353,1.75798121006115,1.40885901027217));
#24439=CARTESIAN_POINT('Ctrl Pts',(-1.49458024744687,1.26369474377317,1.44593424738459));
#24440=CARTESIAN_POINT('Ctrl Pts',(-1.78840024024692,0.916191869184958,
1.47199960088165));
#24441=CARTESIAN_POINT('Ctrl Pts',(-1.94901418738241,0.456060303888852,
1.49806495437871));
#24442=CARTESIAN_POINT('Ctrl Pts',(-1.95278388634516,-0.00168888116712579,
1.52413030787576));
#24443=CARTESIAN_POINT('Origin',(0.,0.,0.));
#24444=CARTESIAN_POINT('',(-1.95720013100772,4.01036975386895E-5,2.32586969212423));
#24445=CARTESIAN_POINT('',(-1.95721475873132,-4.18937055542429E-5,2.22413030787576));
#24446=CARTESIAN_POINT('',(-1.954,-2.39295984553393E-16,0.));
#24447=CARTESIAN_POINT('Ctrl Pts',(-1.95720013100772,4.01036975387313E-5,
2.32586969212423));
#24448=CARTESIAN_POINT('Ctrl Pts',(-1.95720078041499,0.00218844021348119,
2.32574664294735));
#24449=CARTESIAN_POINT('Ctrl Pts',(-1.95719754885173,0.00433677471760079,
2.32562359377048));
#24450=CARTESIAN_POINT('Ctrl Pts',(-1.95719043044659,0.00648509634279326,
2.3255005445936));
#24451=CARTESIAN_POINT('Ctrl Pts',(-1.9550478187754,0.653121371426419,2.28846323116077));
#24452=CARTESIAN_POINT('Ctrl Pts',(-1.60076274017474,1.2985908336322,2.25142591772793));
#24453=CARTESIAN_POINT('Ctrl Pts',(-1.05640644317236,1.64761702679965,2.2143886042951));
#24454=CARTESIAN_POINT('Ctrl Pts',(-0.512050146169983,1.9966432199671,2.17735129086226));
#24455=CARTESIAN_POINT('Ctrl Pts',(0.22237736923411,2.04922614409623,2.14031397742942));
#24456=CARTESIAN_POINT('Ctrl Pts',(0.810904901655155,1.78131122209933,2.10327666399659));
#24457=CARTESIAN_POINT('Ctrl Pts',(1.3994324340762,1.51339630010242,2.06623935056375));
#24458=CARTESIAN_POINT('Ctrl Pts',(1.8420599835142,0.924983531979483,2.02920203713092));
#24459=CARTESIAN_POINT('Ctrl Pts',(1.9363031541186,0.285248202840816,1.99216472369808));
#24460=CARTESIAN_POINT('Ctrl Pts',(2.030546324723,-0.354487126297849,1.95512741026525));
#24461=CARTESIAN_POINT('Ctrl Pts',(1.7764051164938,-1.04554501645225,1.91809009683241));
#24462=CARTESIAN_POINT('Ctrl Pts',(1.29013896790468,-1.47179410874122,1.88105278339957));
#24463=CARTESIAN_POINT('Ctrl Pts',(0.80387281931556,-1.8980432010302,1.84401546996674));
#24464=CARTESIAN_POINT('Ctrl Pts',(0.0854817303665232,-2.05948349545377,
1.8069781565339));
#24465=CARTESIAN_POINT('Ctrl Pts',(-0.536399128085272,-1.88226256360254,
1.76994084310107));
#24466=CARTESIAN_POINT('Ctrl Pts',(-1.15827998653706,-1.70504163175131,
1.73290352966823));
#24467=CARTESIAN_POINT('Ctrl Pts',(-1.68365061449161,-1.18915947362529,
1.69586621623539));
#24468=CARTESIAN_POINT('Ctrl Pts',(-1.87217495490353,-0.570611446107024,
1.65882890280256));
#24469=CARTESIAN_POINT('Ctrl Pts',(-1.92809705865707,-0.387131122580406,
1.64784249924311));
#24470=CARTESIAN_POINT('Ctrl Pts',(-1.95438013781773,-0.194617253664394,
1.63685609568367));
#24471=CARTESIAN_POINT('Ctrl Pts',(-1.95279514498571,-0.00168107824419272,
1.62586969212423));
#24472=CARTESIAN_POINT('Ctrl Pts',(-1.95278388634516,-0.00168888116712579,
1.52413030787576));
#24473=CARTESIAN_POINT('Ctrl Pts',(-1.95437618958592,-0.19503999965723,
1.53514019149113));
#24474=CARTESIAN_POINT('Ctrl Pts',(-1.92798468468382,-0.387966059069047,
1.5461500751065));
#24475=CARTESIAN_POINT('Ctrl Pts',(-1.87182792927594,-0.571799497056349,
1.55715995872187));
#24476=CARTESIAN_POINT('Ctrl Pts',(-1.68272284016263,-1.19084948347563,
1.5942351958343));
#24477=CARTESIAN_POINT('Ctrl Pts',(-1.15608807687694,-1.70679166819193,
1.63131043294672));
#24478=CARTESIAN_POINT('Ctrl Pts',(-0.533290099975553,-1.88316099335306,
1.66838567005915));
#24479=CARTESIAN_POINT('Ctrl Pts',(0.0895078769258353,-2.05953031851418,
1.70546090717157));
#24480=CARTESIAN_POINT('Ctrl Pts',(0.808469067442917,-1.89632678412012,
1.742536144284));
#24481=CARTESIAN_POINT('Ctrl Pts',(1.2940806434107,-1.46834921584087,1.77961138139642));
#24482=CARTESIAN_POINT('Ctrl Pts',(1.77969221937849,-1.04037164756162,1.81668661850885));
#24483=CARTESIAN_POINT('Ctrl Pts',(2.03195418079698,-0.347620045397172,
1.85376185562127));
#24484=CARTESIAN_POINT('Ctrl Pts',(1.93525024356178,0.292404819142093,1.8908370927337));
#24485=CARTESIAN_POINT('Ctrl Pts',(1.83854630632657,0.932429683681362,1.92791232984612));
#24486=CARTESIAN_POINT('Ctrl Pts',(1.39287647043767,1.51972781059545,1.96498756695855));
#24487=CARTESIAN_POINT('Ctrl Pts',(0.802499325163421,1.78512991495868,2.00206280407098));
#24488=CARTESIAN_POINT('Ctrl Pts',(0.212122179889179,2.05053201932191,2.0391380411834));
#24489=CARTESIAN_POINT('Ctrl Pts',(-0.522962274770398,1.99403810113428,
2.07621327829583));
#24490=CARTESIAN_POINT('Ctrl Pts',(-1.06585153299182,1.64154030157863,2.11328851540825));
#24491=CARTESIAN_POINT('Ctrl Pts',(-1.60686689507973,1.29025922210662,2.15023577956409));
#24492=CARTESIAN_POINT('Ctrl Pts',(-1.95701157491646,0.645014173540876,
2.18718304371993));
#24493=CARTESIAN_POINT('Ctrl Pts',(-1.95721475873132,-4.18937055542428E-5,
2.22413030787576));
#24494=CARTESIAN_POINT('Origin',(0.,0.,0.));
#24495=CARTESIAN_POINT('',(-1.95267861104158,0.0016552724044671,3.02586969212423));
#24496=CARTESIAN_POINT('',(-1.95290774954615,0.00171310729769101,2.92413030787577));
#24497=CARTESIAN_POINT('',(-1.954,-2.39295984553393E-16,0.));
#24498=CARTESIAN_POINT('Ctrl Pts',(-1.95267861104158,0.0016552724044671,
3.02586969212423));
#24499=CARTESIAN_POINT('Ctrl Pts',(-1.95426730228936,0.198943040570848,
3.01463719021104));
#24500=CARTESIAN_POINT('Ctrl Pts',(-1.92676912869608,0.39579823972063,3.00340468829784));
#24501=CARTESIAN_POINT('Ctrl Pts',(-1.8683524720406,0.583005555161783,2.99217218638465));
#24502=CARTESIAN_POINT('Ctrl Pts',(-1.67573322844129,1.20029065090429,2.95513487295181));
#24503=CARTESIAN_POINT('Ctrl Pts',(-1.14695545989861,1.71267996796991,2.91809755951898));
#24504=CARTESIAN_POINT('Ctrl Pts',(-0.523913838219462,1.88577589531095,
2.88106024608614));
#24505=CARTESIAN_POINT('Ctrl Pts',(0.0991277834596942,2.05887182265199,
2.84402293265331));
#24506=CARTESIAN_POINT('Ctrl Pts',(0.816433258275323,1.89267436026844,2.80698561922047));
#24507=CARTESIAN_POINT('Ctrl Pts',(1.29986403215874,1.463212197494,2.76994830578763));
#24508=CARTESIAN_POINT('Ctrl Pts',(1.78329480604215,1.03375003471956,2.7329109923548));
#24509=CARTESIAN_POINT('Ctrl Pts',(2.03285087899336,0.341023171554252,2.69587367892196));
#24510=CARTESIAN_POINT('Ctrl Pts',(1.93437033276029,-0.298073569575231,
2.65883636548913));
#24511=CARTESIAN_POINT('Ctrl Pts',(1.83588978652722,-0.93717031070472,2.62179905205629));
#24512=CARTESIAN_POINT('Ctrl Pts',(1.38937262110987,-1.52263692979838,2.58476173862346));
#24513=CARTESIAN_POINT('Ctrl Pts',(0.799082573852251,-1.7866458736405,2.54772442519062));
#24514=CARTESIAN_POINT('Ctrl Pts',(0.208792526594628,-2.05065481748262,
2.51068711175778));
#24515=CARTESIAN_POINT('Ctrl Pts',(-0.525270402503268,-1.99320608607321,
2.47364979832495));
#24516=CARTESIAN_POINT('Ctrl Pts',(-1.06730179468137,-1.64058017638776,
2.43661248489211));
#24517=CARTESIAN_POINT('Ctrl Pts',(-1.60753239434872,-1.28912579681371,
2.39969822063615));
#24518=CARTESIAN_POINT('Ctrl Pts',(-1.95700531140595,-0.644452316926743,
2.36278395638019));
#24519=CARTESIAN_POINT('Ctrl Pts',(-1.95720013100772,4.01036975386895E-5,
2.32586969212423));
#24520=CARTESIAN_POINT('Ctrl Pts',(-1.95721475873132,-4.18937055544587E-5,
2.22413030787576));
#24521=CARTESIAN_POINT('Ctrl Pts',(-1.95721546249205,-0.00227615201876484,
2.22425828083235));
#24522=CARTESIAN_POINT('Ctrl Pts',(-1.9572119680126,-0.00451040806477065,
2.22438625378894));
#24523=CARTESIAN_POINT('Ctrl Pts',(-1.95720426868303,-0.00674464962048316,
2.22451422674553));
#24524=CARTESIAN_POINT('Ctrl Pts',(-1.95497368436953,-0.654030120340289,
2.26158946385795));
#24525=CARTESIAN_POINT('Ctrl Pts',(-1.59981845395926,-1.30009938085624,
2.29866470097038));
#24526=CARTESIAN_POINT('Ctrl Pts',(-1.0545126575596,-1.64884719787949,2.33573993808281));
#24527=CARTESIAN_POINT('Ctrl Pts',(-0.509206861159936,-1.99759501490274,
2.37281517519523));
#24528=CARTESIAN_POINT('Ctrl Pts',(0.226249501229124,-2.04902138843328,
2.40989041230765));
#24529=CARTESIAN_POINT('Ctrl Pts',(0.81478345819529,-1.77955667339696,2.44696564942008));
#24530=CARTESIAN_POINT('Ctrl Pts',(1.40331741516146,-1.51009195836063,2.4840408865325));
#24531=CARTESIAN_POINT('Ctrl Pts',(1.84492896670473,-0.919736154757425,
2.52111612364493));
#24532=CARTESIAN_POINT('Ctrl Pts',(1.93721953774244,-0.279060025103992,
2.55819136075736));
#24533=CARTESIAN_POINT('Ctrl Pts',(2.02951010878015,0.361616104549433,2.59526659786978));
#24534=CARTESIAN_POINT('Ctrl Pts',(1.7724796993123,1.05261256025308,2.63234183498221));
#24535=CARTESIAN_POINT('Ctrl Pts',(1.28393000274363,1.47723315072179,2.66941707209463));
#24536=CARTESIAN_POINT('Ctrl Pts',(0.795380306174951,1.9018537411905,2.70649230920706));
#24537=CARTESIAN_POINT('Ctrl Pts',(0.0753113225054439,2.06009846642426,
2.74356754631949));
#24538=CARTESIAN_POINT('Ctrl Pts',(-0.546256289304822,1.87944090130045,
2.78064278343191));
#24539=CARTESIAN_POINT('Ctrl Pts',(-1.16782390111508,1.69878333617665,2.81771802054433));
#24540=CARTESIAN_POINT('Ctrl Pts',(-1.6908901410661,1.17922348069528,2.85479325765676));
#24541=CARTESIAN_POINT('Ctrl Pts',(-1.875724275851,0.558885028961709,2.89186849476918));
#24542=CARTESIAN_POINT('Ctrl Pts',(-1.92933673865706,0.37895142411412,2.90262243247138));
#24543=CARTESIAN_POINT('Ctrl Pts',(-1.95449266845916,0.190538998342851,
2.91337637017357));
#24544=CARTESIAN_POINT('Ctrl Pts',(-1.95290774954615,0.00171310729769108,
2.92413030787576));
#24545=CARTESIAN_POINT('Origin',(0.,0.,0.));
#24546=CARTESIAN_POINT('',(-1.95135045472565,-0.00103665430809308,3.72586969212423));
#24547=CARTESIAN_POINT('',(-1.95115009645722,-0.000862413589311458,3.62413030787577));
#24548=CARTESIAN_POINT('',(-1.954,-2.39295984553393E-16,0.));
#24549=CARTESIAN_POINT('Ctrl Pts',(-1.95135045472565,-0.00103665430809308,
3.72586969212423));
#24550=CARTESIAN_POINT('Ctrl Pts',(-1.94945762145185,0.39205003232945,3.70352773747472));
#24551=CARTESIAN_POINT('Ctrl Pts',(-1.83432541049109,0.786156754205215,
3.6811857828252));
#24552=CARTESIAN_POINT('Ctrl Pts',(-1.61355237927334,1.1077387582254,3.65884382817569));
#24553=CARTESIAN_POINT('Ctrl Pts',(-1.2475664983152,1.64084043460512,3.62180651474286));
#24554=CARTESIAN_POINT('Ctrl Pts',(-0.591266345378013,1.97463505701166,
3.58476920131002));
#24555=CARTESIAN_POINT('Ctrl Pts',(0.0551170192794968,1.95642494139715,
3.54773188787719));
#24556=CARTESIAN_POINT('Ctrl Pts',(0.701500383937021,1.93821482578265,3.51069457444435));
#24557=CARTESIAN_POINT('Ctrl Pts',(1.33796696031487,1.56799997214707,3.47365726101151));
#24558=CARTESIAN_POINT('Ctrl Pts',(1.67335875584854,1.01513886309221,3.43661994757868));
#24559=CARTESIAN_POINT('Ctrl Pts',(2.00875055138221,0.46227775403734,3.39958263414584));
#24560=CARTESIAN_POINT('Ctrl Pts',(2.04306756607169,-0.273229610436822,
3.36254532071301));
#24561=CARTESIAN_POINT('Ctrl Pts',(1.76061113877997,-0.854918040011614,
3.32550800728017));
#24562=CARTESIAN_POINT('Ctrl Pts',(1.47815471148825,-1.4366064695864,3.28847069384734));
#24563=CARTESIAN_POINT('Ctrl Pts',(0.878924842215338,-1.86447596426182,
3.2514333804145));
#24564=CARTESIAN_POINT('Ctrl Pts',(0.237045219929842,-1.94279335001325,
3.21439606698166));
#24565=CARTESIAN_POINT('Ctrl Pts',(-0.404834402355659,-2.02111073576468,
3.17735875354883));
#24566=CARTESIAN_POINT('Ctrl Pts',(-1.08936377765374,-1.74987601259212,
3.14032144011599));
#24567=CARTESIAN_POINT('Ctrl Pts',(-1.50339810597481,-1.25316821379613,
3.10328412668316));
#24568=CARTESIAN_POINT('Ctrl Pts',(-1.79186605396357,-0.907099615934405,
3.07747931516352));
#24569=CARTESIAN_POINT('Ctrl Pts',(-1.94902885620257,-0.451580677342798,
3.05167450364387));
#24570=CARTESIAN_POINT('Ctrl Pts',(-1.95267861104158,0.0016552724044671,
3.02586969212423));
#24571=CARTESIAN_POINT('Ctrl Pts',(-1.95290774954615,0.00171310729769101,
2.92413030787577));
#24572=CARTESIAN_POINT('Ctrl Pts',(-1.94902850769025,-0.460456467442357,
2.950451607286));
#24573=CARTESIAN_POINT('Ctrl Pts',(-1.78495210853218,-0.925103000270984,
2.97677290669623));
#24574=CARTESIAN_POINT('Ctrl Pts',(-1.48583543343396,-1.27396510910143,
3.00309420610646));
#24575=CARTESIAN_POINT('Ctrl Pts',(-1.06451042661324,-1.76535974744522,
3.04016944321889));
#24576=CARTESIAN_POINT('Ctrl Pts',(-0.375258383353002,-2.02703197614702,
3.07724468033131));
#24577=CARTESIAN_POINT('Ctrl Pts',(0.266023999143107,-1.93905267245523,
3.11431991744374));
#24578=CARTESIAN_POINT('Ctrl Pts',(0.907306381639212,-1.85107336876345,
3.15139515455616));
#24579=CARTESIAN_POINT('Ctrl Pts',(1.50061910337119,-1.4134425326781,3.18847039166859));
#24580=CARTESIAN_POINT('Ctrl Pts',(1.77403619606301,-0.826734304146555,
3.22554562878102));
#24581=CARTESIAN_POINT('Ctrl Pts',(2.04745328875484,-0.240026075615009,
3.26262086589344));
#24582=CARTESIAN_POINT('Ctrl Pts',(2.0009747524065,0.495759545362725,3.29969610300586));
#24583=CARTESIAN_POINT('Ctrl Pts',(1.65590254220004,1.04339867994717,3.33677134011829));
#24584=CARTESIAN_POINT('Ctrl Pts',(1.31083033199357,1.59103781453161,3.37384657723071));
#24585=CARTESIAN_POINT('Ctrl Pts',(0.667164447928974,1.95053046272276,3.41092181434314));
#24586=CARTESIAN_POINT('Ctrl Pts',(0.0199086246964731,1.9571146316129,3.44799705145557));
#24587=CARTESIAN_POINT('Ctrl Pts',(-0.627347198536033,1.96369880050304,
3.485072288568));
#24588=CARTESIAN_POINT('Ctrl Pts',(-1.27819296093644,1.61737449009216,3.52214752568042));
#24589=CARTESIAN_POINT('Ctrl Pts',(-1.63433425949862,1.07686840552899,3.55922276279284));
#24590=CARTESIAN_POINT('Ctrl Pts',(-1.8421662177247,0.761447423909083,3.58085861115382));
#24591=CARTESIAN_POINT('Ctrl Pts',(-1.94963677903995,0.379897976317775,
3.60249445951479));
#24592=CARTESIAN_POINT('Ctrl Pts',(-1.95115009645722,-0.000862413589311458,
3.62413030787577));
#24593=CARTESIAN_POINT('Origin',(0.,0.,0.));
#24594=CARTESIAN_POINT('',(-1.95645463735042,-0.00107680116258307,4.42586969212423));
#24595=CARTESIAN_POINT('',(-1.9560689354221,-0.00131000797615835,4.32413030787576));
#24596=CARTESIAN_POINT('',(-1.954,-2.39295984553393E-16,0.));
#24597=CARTESIAN_POINT('Ctrl Pts',(-1.95645463735042,-0.00107680116258307,
4.42586969212423));
#24598=CARTESIAN_POINT('Ctrl Pts',(-1.95257837355362,0.583548870363389,
4.3924182847384));
#24599=CARTESIAN_POINT('Ctrl Pts',(-1.67319437992126,1.17138871222795,4.35896687735257));
#24600=CARTESIAN_POINT('Ctrl Pts',(-1.21542355114692,1.53407367113183,4.32551546996674));
#24601=CARTESIAN_POINT('Ctrl Pts',(-0.70858085032514,1.93563753794803,4.2884781565339));
#24602=CARTESIAN_POINT('Ctrl Pts',(0.0169438143861521,2.0611871352921,4.25144084310107));
#24603=CARTESIAN_POINT('Ctrl Pts',(0.629251938590984,1.85328854601076,4.21440352966823));
#24604=CARTESIAN_POINT('Ctrl Pts',(1.24156006279581,1.64538995672942,4.1773662162354));
#24605=CARTESIAN_POINT('Ctrl Pts',(1.74065164649418,1.10404318082267,4.14032890280256));
#24606=CARTESIAN_POINT('Ctrl Pts',(1.89821225955213,0.476892707953959,4.10329158936972));
#24607=CARTESIAN_POINT('Ctrl Pts',(2.05577287261007,-0.15025776491475,4.06625427593688));
#24608=CARTESIAN_POINT('Ctrl Pts',(1.87180251502759,-0.86321193474541,4.02921696250405));
#24609=CARTESIAN_POINT('Ctrl Pts',(1.4304602644841,-1.33582179532369,3.99217964907122));
#24610=CARTESIAN_POINT('Ctrl Pts',(0.989118013940611,-1.80843165590198,
3.95514233563838));
#24611=CARTESIAN_POINT('Ctrl Pts',(0.290403870436121,-2.04069720722789,
3.91810502220554));
#24612=CARTESIAN_POINT('Ctrl Pts',(-0.346048402169674,-1.92636625294191,
3.88106770877271));
#24613=CARTESIAN_POINT('Ctrl Pts',(-0.982500674775478,-1.81203529865592,
3.84403039533987));
#24614=CARTESIAN_POINT('Ctrl Pts',(-1.55669107648259,-1.35110783875803,
3.80699308190704));
#24615=CARTESIAN_POINT('Ctrl Pts',(-1.80595047284659,-0.754439743632632,
3.7699557684742));
#24616=CARTESIAN_POINT('Ctrl Pts',(-1.9048495538052,-0.517698713581134,
3.75526040969088));
#24617=CARTESIAN_POINT('Ctrl Pts',(-1.95259546056833,-0.259588333590661,
3.74056505090755));
#24618=CARTESIAN_POINT('Ctrl Pts',(-1.95135045472565,-0.00103665430809308,
3.72586969212423));
#24619=CARTESIAN_POINT('Ctrl Pts',(-1.95115009645722,-0.000862413589311458,
3.62413030787577));
#24620=CARTESIAN_POINT('Ctrl Pts',(-1.95223000307885,-0.272573861314833,
3.63956969662722));
#24621=CARTESIAN_POINT('Ctrl Pts',(-1.89935350538763,-0.543883498707529,
3.65500908537867));
#24622=CARTESIAN_POINT('Ctrl Pts',(-1.79048714938831,-0.790474416076489,
3.67044847413012));
#24623=CARTESIAN_POINT('Ctrl Pts',(-1.52906190599187,-1.38262329440335,
3.70752371124255));
#24624=CARTESIAN_POINT('Ctrl Pts',(-0.944774584475045,-1.83223319234163,
3.74459894835497));
#24625=CARTESIAN_POINT('Ctrl Pts',(-0.305414648672952,-1.93323974896447,
3.7816741854674));
#24626=CARTESIAN_POINT('Ctrl Pts',(0.333945287129141,-2.0342463055873,3.81874942257982));
#24627=CARTESIAN_POINT('Ctrl Pts',(1.0283778372165,-1.7866495208947,3.85582465969225));
#24628=CARTESIAN_POINT('Ctrl Pts',(1.45961198421181,-1.30392748653653,3.89289989680467));
#24629=CARTESIAN_POINT('Ctrl Pts',(1.89084613120712,-0.821205452178361,
3.9299751339171));
#24630=CARTESIAN_POINT('Ctrl Pts',(2.05888187511037,-0.103358168154617,
3.96705037102952));
#24631=CARTESIAN_POINT('Ctrl Pts',(1.88670539052006,0.520611951436678,4.00412560814195));
#24632=CARTESIAN_POINT('Ctrl Pts',(1.71452890592974,1.14458207102797,4.04120084525437));
#24633=CARTESIAN_POINT('Ctrl Pts',(1.20214019284586,1.67467502618682,4.0782760823668));
#24634=CARTESIAN_POINT('Ctrl Pts',(0.58437628040953,1.8679396129137,4.11535131947923));
#24635=CARTESIAN_POINT('Ctrl Pts',(-0.0333876320267997,2.06120419964058,
4.15242655659165));
#24636=CARTESIAN_POINT('Ctrl Pts',(-0.756526743815583,1.9176404179355,4.18950179370408));
#24637=CARTESIAN_POINT('Ctrl Pts',(-1.25361330032381,1.50304614961146,4.2265770308165));
#24638=CARTESIAN_POINT('Ctrl Pts',(-1.68959543059256,1.13941593283223,4.25909478983626));
#24639=CARTESIAN_POINT('Ctrl Pts',(-1.95168429546986,0.567292711935832,
4.29161254885601));
#24640=CARTESIAN_POINT('Ctrl Pts',(-1.9560689354221,-0.00131000797615835,
4.32413030787576));
#24641=CARTESIAN_POINT('Origin',(0.,0.,0.));
#24642=CARTESIAN_POINT('',(-1.95458552907139,0.00173412683576277,5.12586969212423));
#24643=CARTESIAN_POINT('',(-1.9552206747184,0.00161939276430114,5.02413030787577));
#24644=CARTESIAN_POINT('',(-1.954,-2.39295984553393E-16,0.));
#24645=CARTESIAN_POINT('Ctrl Pts',(-1.95458552907139,0.00173412683576277,
5.12586969212423));
#24646=CARTESIAN_POINT('Ctrl Pts',(-1.95579889273049,0.133549336413818,
5.11834614543492));
#24647=CARTESIAN_POINT('Ctrl Pts',(-1.94360248016884,0.265141296927549,
5.11082259874561));
#24648=CARTESIAN_POINT('Ctrl Pts',(-1.91717253101555,0.393809524200435,
5.10329905205629));
#24649=CARTESIAN_POINT('Ctrl Pts',(-1.78706177989932,1.02722427646379,5.06626173862345));
#24650=CARTESIAN_POINT('Ctrl Pts',(-1.31200866513269,1.58978387278703,5.02922442519062));
#24651=CARTESIAN_POINT('Ctrl Pts',(-0.709330998225857,1.82413979092323,
4.99218711175778));
#24652=CARTESIAN_POINT('Ctrl Pts',(-0.106653331319023,2.05849570905944,
4.95514979832495));
#24653=CARTESIAN_POINT('Ctrl Pts',(0.623648887728016,1.96464794900861,4.91811248489211));
#24654=CARTESIAN_POINT('Ctrl Pts',(1.14749162443816,1.58552811433593,4.88107517145928));
#24655=CARTESIAN_POINT('Ctrl Pts',(1.67133436114829,1.20640827966324,4.84403785802644));
#24656=CARTESIAN_POINT('Ctrl Pts',(1.98871761552153,0.542016370368706,4.8070005445936));
#24657=CARTESIAN_POINT('Ctrl Pts',(1.95445124244436,-0.103714902901561,
4.76996323116077));
#24658=CARTESIAN_POINT('Ctrl Pts',(1.9201848693672,-0.749446176171828,4.73292591772793));
#24659=CARTESIAN_POINT('Ctrl Pts',(1.53426886883963,-1.37651681341782,4.6958886042951));
#24660=CARTESIAN_POINT('Ctrl Pts',(0.973244372713117,-1.69806708597997,
4.65885129086226));
#24661=CARTESIAN_POINT('Ctrl Pts',(0.412219876586598,-2.01961735854213,
4.62181397742943));
#24662=CARTESIAN_POINT('Ctrl Pts',(-0.323913115138867,-2.03564726642044,
4.58477666399659));
#24663=CARTESIAN_POINT('Ctrl Pts',(-0.898403214163087,-1.7388237693533,
4.54773935056375));
#24664=CARTESIAN_POINT('Ctrl Pts',(-1.4728933131873,-1.44200027228616,4.51070203713092));
#24665=CARTESIAN_POINT('Ctrl Pts',(-1.88574051951028,-0.832323370273586,
4.47366472369808));
#24666=CARTESIAN_POINT('Ctrl Pts',(-1.94808375420563,-0.188695851123138,
4.43662741026525));
#24667=CARTESIAN_POINT('Ctrl Pts',(-1.95411974768256,-0.126380645212594,
4.43304150421824));
#24668=CARTESIAN_POINT('Ctrl Pts',(-1.95687016300016,-0.0637471906795113,
4.42945559817124));
#24669=CARTESIAN_POINT('Ctrl Pts',(-1.95645463735042,-0.00107680116258307,
4.42586969212423));
#24670=CARTESIAN_POINT('Ctrl Pts',(-1.9560689354221,-0.00131000797615835,
4.32413030787576));
#24671=CARTESIAN_POINT('Ctrl Pts',(-1.95668345810536,-0.0810016754695383,
4.32868778596844));
#24672=CARTESIAN_POINT('Ctrl Pts',(-1.95223589499426,-0.160624189738801,
4.33324526406111));
#24673=CARTESIAN_POINT('Ctrl Pts',(-1.94249551147141,-0.239593869899598,
4.33780274215378));
#24674=CARTESIAN_POINT('Ctrl Pts',(-1.86325716488311,-0.882014866143589,
4.3748779792662));
#24675=CARTESIAN_POINT('Ctrl Pts',(-1.43374647047883,-1.48123210368856,
4.41195321637863));
#24676=CARTESIAN_POINT('Ctrl Pts',(-0.850815960071711,-1.76261346774659,
4.44902845349105));
#24677=CARTESIAN_POINT('Ctrl Pts',(-0.267885449664584,-2.04399483180463,
4.48610369060348));
#24678=CARTESIAN_POINT('Ctrl Pts',(0.468464876745396,-2.00754032237573,
4.52317892771591));
#24679=CARTESIAN_POINT('Ctrl Pts',(1.02075232548754,-1.66995770146661,4.56025416482833));
#24680=CARTESIAN_POINT('Ctrl Pts',(1.57303977422969,-1.3323750805575,4.59732940194076));
#24681=CARTESIAN_POINT('Ctrl Pts',(1.941264345304,-0.693664348168167,4.63440463905318));
#24682=CARTESIAN_POINT('Ctrl Pts',(1.95666204750888,-0.0465582032952289,
4.67147987616561));
#24683=CARTESIAN_POINT('Ctrl Pts',(1.97205974971376,0.6005479415777,4.70855511327803));
#24684=CARTESIAN_POINT('Ctrl Pts',(1.63463058304921,1.25604949893424,4.74563035039046));
#24685=CARTESIAN_POINT('Ctrl Pts',(1.09902444690466,1.61951823074648,4.78270558750289));
#24686=CARTESIAN_POINT('Ctrl Pts',(0.56341831076011,1.98298696255872,4.81978082461531));
#24687=CARTESIAN_POINT('Ctrl Pts',(-0.170364794864445,2.05442286882665,
4.85685606172773));
#24688=CARTESIAN_POINT('Ctrl Pts',(-0.766018779707725,1.80108557937185,
4.89393129884016));
#24689=CARTESIAN_POINT('Ctrl Pts',(-1.361672764551,1.54774828991705,4.93100653595259));
#24690=CARTESIAN_POINT('Ctrl Pts',(-1.81919762861299,0.96963780473953,4.96808177306502));
#24691=CARTESIAN_POINT('Ctrl Pts',(-1.92890143946537,0.331712632206103,
5.00515701017744));
#24692=CARTESIAN_POINT('Ctrl Pts',(-1.9476151256888,0.222892971156397,5.01148144274355));
#24693=CARTESIAN_POINT('Ctrl Pts',(-1.95620763248682,0.112332773766476,
5.01780587530966));
#24694=CARTESIAN_POINT('Ctrl Pts',(-1.9552206747184,0.00161939276430114,
5.02413030787577));
#24695=CARTESIAN_POINT('Origin',(0.,0.,0.));
#24696=CARTESIAN_POINT('',(-1.95079790389112,-3.269510144494E-5,5.82586969212423));
#24697=CARTESIAN_POINT('',(-1.95085192255358,0.000383174536113729,5.72413030787576));
#24698=CARTESIAN_POINT('',(-1.954,-2.39295984553393E-16,0.));
#24699=CARTESIAN_POINT('Ctrl Pts',(-1.95079807093469,-3.26933958413878E-5,
5.82586969212423));
#24700=CARTESIAN_POINT('Ctrl Pts',(-1.95074883721548,0.328029941286317,
5.8072366926986));
#24701=CARTESIAN_POINT('Ctrl Pts',(-1.87242650231768,0.656114687980161,
5.78860369327296));
#24702=CARTESIAN_POINT('Ctrl Pts',(-1.71596284018057,0.941333347646706,
5.76997069384733));
#24703=CARTESIAN_POINT('Ctrl Pts',(-1.40495581640267,1.50827013831881,5.7329333804145));
#24704=CARTESIAN_POINT('Ctrl Pts',(-0.785207871169114,1.90584052998572,
5.69589606698167));
#24705=CARTESIAN_POINT('Ctrl Pts',(-0.140229809906548,1.95217121547304,
5.65885875354883));
#24706=CARTESIAN_POINT('Ctrl Pts',(0.504748251356019,1.99850190096035,5.62182144011599));
#24707=CARTESIAN_POINT('Ctrl Pts',(1.1749564286476,1.69359288026805,5.58478412668316));
#24708=CARTESIAN_POINT('Ctrl Pts',(1.56380177877164,1.17692822962597,5.54774681325032));
#24709=CARTESIAN_POINT('Ctrl Pts',(1.95264712889569,0.660263578983889,5.51070949981748));
#24710=CARTESIAN_POINT('Ctrl Pts',(2.06012965185219,-0.068156701607988,
5.47367218638465));
#24711=CARTESIAN_POINT('Ctrl Pts',(1.83708014107304,-0.675109688693547,
5.43663487295181));
#24712=CARTESIAN_POINT('Ctrl Pts',(1.61403063029389,-1.2820626757791,5.39959755951898));
#24713=CARTESIAN_POINT('Ctrl Pts',(1.06044908577908,-1.76754836935834,5.36256024608614));
#24714=CARTESIAN_POINT('Ctrl Pts',(0.429577047133733,-1.90947637973667,
5.32552293265331));
#24715=CARTESIAN_POINT('Ctrl Pts',(-0.201294991511623,-2.051404390115,5.28848561922047));
#24716=CARTESIAN_POINT('Ctrl Pts',(-0.909457524287529,-1.84977471729243,
5.25144830578764));
#24717=CARTESIAN_POINT('Ctrl Pts',(-1.37095459694257,-1.39682492677941,
5.2144109923548));
#24718=CARTESIAN_POINT('Ctrl Pts',(-1.73870581031982,-1.03588474984214,
5.18489722561128));
#24719=CARTESIAN_POINT('Ctrl Pts',(-1.94982568195559,-0.515357546731067,
5.15538345886775));
#24720=CARTESIAN_POINT('Ctrl Pts',(-1.95458552907139,0.00173412683576277,
5.12586969212423));
#24721=CARTESIAN_POINT('Ctrl Pts',(-1.9552206747184,0.00161939276430114,
5.02413030787577));
#24722=CARTESIAN_POINT('Ctrl Pts',(-1.95042186547898,-0.536693808344559,
5.05488111242208));
#24723=CARTESIAN_POINT('Ctrl Pts',(-1.71915285367837,-1.07862845650355,
5.0856319169684));
#24724=CARTESIAN_POINT('Ctrl Pts',(-1.32368315644793,-1.44172013107889,
5.11638272151471));
#24725=CARTESIAN_POINT('Ctrl Pts',(-0.846878304935377,-1.87948786194111,
5.15345795862714));
#24726=CARTESIAN_POINT('Ctrl Pts',(-0.131385844267519,-2.0572834637762,
5.19053319573957));
#24727=CARTESIAN_POINT('Ctrl Pts',(0.494871066573067,-1.89361998960963,
5.22760843285199));
#24728=CARTESIAN_POINT('Ctrl Pts',(1.12112797741365,-1.72995651544305,5.26468366996442));
#24729=CARTESIAN_POINT('Ctrl Pts',(1.65814933842698,-1.22483396527481,5.30175890707684));
#24730=CARTESIAN_POINT('Ctrl Pts',(1.85980853758091,-0.609759157741489,
5.33883414418927));
#24731=CARTESIAN_POINT('Ctrl Pts',(2.06146773673485,0.00531564979182955,
5.37590938130169));
#24732=CARTESIAN_POINT('Ctrl Pts',(1.9277647740294,0.730342714690214,5.41298461841412));
#24733=CARTESIAN_POINT('Ctrl Pts',(1.51997812810125,1.23302900604299,5.45005985552654));
#24734=CARTESIAN_POINT('Ctrl Pts',(1.11219148217311,1.73571529739576,5.48713509263897));
#24735=CARTESIAN_POINT('Ctrl Pts',(0.430321153022272,2.01606081520293,5.52421032975139));
#24736=CARTESIAN_POINT('Ctrl Pts',(-0.213119314048168,1.94557811718459,
5.56128556686382));
#24737=CARTESIAN_POINT('Ctrl Pts',(-0.856559781118622,1.87509541916625,
5.59836080397625));
#24738=CARTESIAN_POINT('Ctrl Pts',(-1.46157038610868,1.45378450532239,5.63543604108868));
#24739=CARTESIAN_POINT('Ctrl Pts',(-1.75086384963453,0.874739824296975,
5.6725112782011));
#24740=CARTESIAN_POINT('Ctrl Pts',(-1.88512280557994,0.606009472173862,
5.68971762142599));
#24741=CARTESIAN_POINT('Ctrl Pts',(-1.95138199037298,0.30330611490569,5.70692396465088));
#24742=CARTESIAN_POINT('Ctrl Pts',(-1.95085192255358,0.000383174536113729,
5.72413030787576));
#24743=CARTESIAN_POINT('Origin',(0.,0.,0.));
#24744=CARTESIAN_POINT('',(-1.95467666345581,-0.00169153748172557,6.52586969212423));
#24745=CARTESIAN_POINT('',(-1.95381346134878,-0.0017935399644829,6.42413030787577));
#24746=CARTESIAN_POINT('',(-1.954,-2.39295984553393E-16,0.));
#24747=CARTESIAN_POINT('Ctrl Pts',(-1.95467666345581,-0.00169153748172557,
6.52586969212423));
#24748=CARTESIAN_POINT('Ctrl Pts',(-1.94989845242835,0.519322657074601,
6.49612723996228));
#24749=CARTESIAN_POINT('Ctrl Pts',(-1.7351643372623,1.04378980187726,6.46638478780033));
#24750=CARTESIAN_POINT('Ctrl Pts',(-1.36233982826997,1.40523012754949,6.43664233563838));
#24751=CARTESIAN_POINT('Ctrl Pts',(-0.898073529048792,1.85532007158963,
6.39960502220555));
#24752=CARTESIAN_POINT('Ctrl Pts',(-0.188657797713761,2.05260571068844,
6.36256770877271));
#24753=CARTESIAN_POINT('Ctrl Pts',(0.441334197613014,1.90680041588618,6.32553039533987));
#24754=CARTESIAN_POINT('Ctrl Pts',(1.07132619293978,1.76099512108392,6.28849308190704));
#24755=CARTESIAN_POINT('Ctrl Pts',(1.62189445225829,1.2720988923806,6.2514557684742));
#24756=CARTESIAN_POINT('Ctrl Pts',(1.84119904752624,0.663781270447278,6.21441845504137));
#24757=CARTESIAN_POINT('Ctrl Pts',(2.06050364279419,0.055463648513944,6.17738114160853));
#24758=CARTESIAN_POINT('Ctrl Pts',(1.94854457401157,-0.672275366649399,
6.14034382817569));
#24759=CARTESIAN_POINT('Ctrl Pts',(1.556526550614,-1.18653430832568,6.10330651474286));
#24760=CARTESIAN_POINT('Ctrl Pts',(1.16450852721644,-1.70079325000195,6.06626920131002));
#24761=CARTESIAN_POINT('Ctrl Pts',(0.492431549203928,-2.00157211819116,
6.02923188787718));
#24762=CARTESIAN_POINT('Ctrl Pts',(-0.152249713101387,-1.9512713582857,
5.99219457444435));
#24763=CARTESIAN_POINT('Ctrl Pts',(-0.796930975406703,-1.90097059838025,
5.95515726101152));
#24764=CARTESIAN_POINT('Ctrl Pts',(-1.41421652200483,-1.49959021038012,
5.91811994757868));
#24765=CARTESIAN_POINT('Ctrl Pts',(-1.72172624414277,-0.930748421541415,
5.88108263414585));
#24766=CARTESIAN_POINT('Ctrl Pts',(-1.87453175193852,-0.648083672620247,
5.86267832013864));
#24767=CARTESIAN_POINT('Ctrl Pts',(-1.95084670040156,-0.324068969295429,
5.84427400613143));
#24768=CARTESIAN_POINT('Ctrl Pts',(-1.95079807093469,-3.26933958413878E-5,
5.82586969212423));
#24769=CARTESIAN_POINT('Ctrl Pts',(-1.95085192255358,0.000383174536113729,
5.72413030787576));
#24770=CARTESIAN_POINT('Ctrl Pts',(-1.95023983077328,-0.349414785416059,
5.7439992017633));
#24771=CARTESIAN_POINT('Ctrl Pts',(-1.86056894683247,-0.699505544060014,
5.76386809565083));
#24772=CARTESIAN_POINT('Ctrl Pts',(-1.68370318859703,-0.997916657928721,
5.78373698953837));
#24773=CARTESIAN_POINT('Ctrl Pts',(-1.35367274197203,-1.55475001092207,
5.82081222665079));
#24774=CARTESIAN_POINT('Ctrl Pts',(-0.7200355266604,-1.9316382687018,5.85788746376322));
#24775=CARTESIAN_POINT('Ctrl Pts',(-0.0731991044283191,-1.95584662548515,
5.89496270087565));
#24776=CARTESIAN_POINT('Ctrl Pts',(0.573637317803748,-1.9800549822685,5.93203793798808));
#24777=CARTESIAN_POINT('Ctrl Pts',(1.23367294695625,-1.65158343805548,5.9691131751005));
#24778=CARTESIAN_POINT('Ctrl Pts',(1.60440177887889,-1.12097662310535,6.00618841221292));
#24779=CARTESIAN_POINT('Ctrl Pts',(1.97513061080152,-0.590369808155209,
6.04326364932535));
#24780=CARTESIAN_POINT('Ctrl Pts',(2.05655264549427,0.142372277532039,6.08033888643777));
#24781=CARTESIAN_POINT('Ctrl Pts',(1.81135015364285,0.741420988743503,6.1174141235502));
#24782=CARTESIAN_POINT('Ctrl Pts',(1.56614766179142,1.34046969995497,6.15448936066263));
#24783=CARTESIAN_POINT('Ctrl Pts',(0.994320643395809,1.80582503669066,6.19156459777505));
#24784=CARTESIAN_POINT('Ctrl Pts',(0.357948800551169,1.92420559652088,6.22863983488748));
#24785=CARTESIAN_POINT('Ctrl Pts',(-0.278423042293462,2.04258615635109,
6.2657150719999));
#24786=CARTESIAN_POINT('Ctrl Pts',(-0.97933970958712,1.81399193927586,6.30279030911233));
#24787=CARTESIAN_POINT('Ctrl Pts',(-1.42356034057997,1.34319300038089,6.33986554622475));
#24788=CARTESIAN_POINT('Ctrl Pts',(-1.76010254058954,0.986515035416152,
6.36795380010842));
#24789=CARTESIAN_POINT('Ctrl Pts',(-1.9493114895094,0.49082125388787,6.3960420539921));
#24790=CARTESIAN_POINT('Ctrl Pts',(-1.95381346134878,-0.0017935399644829,
6.42413030787577));
#24791=CARTESIAN_POINT('Origin',(0.,0.,-1.2940562256037));
#24792=CARTESIAN_POINT('',(-1.55603866428123,-0.00134656425434549,6.75594377439631));
#24793=CARTESIAN_POINT('',(-1.55791343064937,0.000503462391539915,6.89405622560371));
#24794=CARTESIAN_POINT('',(-1.5555,-9.09151186476045E-14,-1.2940562256037));
#24795=CARTESIAN_POINT('',(-1.54730100999696,0.15949869736893,7.4445));
#24796=CARTESIAN_POINT('Ctrl Pts',(-1.55603866428123,-0.00134656425434554,
6.7559437743963));
#24797=CARTESIAN_POINT('Ctrl Pts',(-1.55697159855378,-0.103073339358787,
6.76323863566719));
#24798=CARTESIAN_POINT('Ctrl Pts',(-1.50153911503434,-0.720280229157285,
6.80757081037091));
#24799=CARTESIAN_POINT('Ctrl Pts',(-0.676946582872774,-1.70937536089767,
6.88894029850746));
#24800=CARTESIAN_POINT('Ctrl Pts',(1.06890459630572,-1.49565296874813,7.00005223880597));
#24801=CARTESIAN_POINT('Ctrl Pts',(1.83584092749207,0.0856835708872964,
7.11116417910447));
#24802=CARTESIAN_POINT('Ctrl Pts',(0.924965623038614,1.59014055343882,7.22227611940298));
#24803=CARTESIAN_POINT('Ctrl Pts',(-0.835858495286665,1.63675999125994,
7.33338805970149));
#24804=CARTESIAN_POINT('Ctrl Pts',(-1.49427628245053,0.673892957891604,
7.40746268656716));
#24805=CARTESIAN_POINT('Ctrl Pts',(-1.54730100999696,0.159498697368912,
7.4445));
#24806=CARTESIAN_POINT('',(-0.352169241380506,1.51510959188617,7.4445));
#24807=CARTESIAN_POINT('Origin',(0.,0.,7.4445));
#24808=CARTESIAN_POINT('Ctrl Pts',(-1.55791343064937,0.000503462391539858,
6.8940562256037));
#24809=CARTESIAN_POINT('Ctrl Pts',(-1.55587997194015,-0.488621135891717,
6.9292365352861));
#24810=CARTESIAN_POINT('Ctrl Pts',(-1.04365545248604,-1.49691459517969,
7.00149208208092));
#24811=CARTESIAN_POINT('Ctrl Pts',(0.672826183539381,-1.71093187207897,
7.11082286598819));
#24812=CARTESIAN_POINT('Ctrl Pts',(1.80435891657647,-0.361603954366771,
7.22204857732544));
#24813=CARTESIAN_POINT('Ctrl Pts',(1.27791236939833,1.32169962363241,7.33327428866273));
#24814=CARTESIAN_POINT('Ctrl Pts',(0.152038852759137,1.63230677878407,7.40742476288758));
#24815=CARTESIAN_POINT('Ctrl Pts',(-0.352169241380528,1.51510959188617,
7.44450000000001));
#24816=CARTESIAN_POINT('Origin',(0.,0.,-1.2940562256037));
#24817=CARTESIAN_POINT('',(-1.5529510743802,-2.6025883987463E-5,6.0559437743963));
#24818=CARTESIAN_POINT('',(-1.55535150415969,-0.0014277642860383,6.1940562256037));
#24819=CARTESIAN_POINT('',(-1.5555,-9.09151186476045E-14,-1.2940562256037));
#24820=CARTESIAN_POINT('Ctrl Pts',(-1.5529510743802,-2.60258839871949E-5,
6.0559437743963));
#24821=CARTESIAN_POINT('Ctrl Pts',(-1.55298978632273,-0.257978138044578,
6.07434808840351));
#24822=CARTESIAN_POINT('Ctrl Pts',(-1.36998122495718,-1.03498796260698,
6.12978971584355));
#24823=CARTESIAN_POINT('Ctrl Pts',(-0.143008426055117,-1.83280806515592,
6.2222686567164));
#24824=CARTESIAN_POINT('Ctrl Pts',(1.4620310918033,-1.11449456034272,6.33338059701493));
#24825=CARTESIAN_POINT('Ctrl Pts',(1.72940928754233,0.623475815429911,6.44449253731343));
#24826=CARTESIAN_POINT('Ctrl Pts',(0.414554230167772,1.79104708014026,6.55560447761194));
#24827=CARTESIAN_POINT('Ctrl Pts',(-1.16842639544942,1.35082658514471,6.65942155663957));
#24828=CARTESIAN_POINT('Ctrl Pts',(-1.55223492464296,0.413411664830818,
6.72620132223435));
#24829=CARTESIAN_POINT('Ctrl Pts',(-1.55603866428123,-0.00134656425434554,
6.7559437743963));
#24830=CARTESIAN_POINT('Ctrl Pts',(-1.55535150415969,-0.00142776428603842,
6.1940562256037));
#24831=CARTESIAN_POINT('Ctrl Pts',(-1.55649817143771,-0.126898399140172,
6.20304320883246));
#24832=CARTESIAN_POINT('Ctrl Pts',(-1.48522496230459,-0.768704224613979,
6.24910542917363));
#24833=CARTESIAN_POINT('Ctrl Pts',(-0.59667036110871,-1.73952595846347,
6.33224288662724));
#24834=CARTESIAN_POINT('Ctrl Pts',(1.13899278941852,-1.44381691390763,6.44346859796452));
#24835=CARTESIAN_POINT('Ctrl Pts',(1.83065601360088,0.17532136832598,6.5546943093018));
#24836=CARTESIAN_POINT('Ctrl Pts',(0.844193344579619,1.63380261073593,6.66592002063907));
#24837=CARTESIAN_POINT('Ctrl Pts',(-0.915934603694247,1.5945880622222,6.77714573197635));
#24838=CARTESIAN_POINT('Ctrl Pts',(-1.5455164129256,0.568558209121068,6.85319113363123));
#24839=CARTESIAN_POINT('Ctrl Pts',(-1.55802295943751,0.0268493253573782,
6.89216129817368));
#24840=CARTESIAN_POINT('Ctrl Pts',(-1.55791343064937,0.000503462391539858,
6.8940562256037));
#24841=CARTESIAN_POINT('Origin',(0.,0.,-1.2940562256037));
#24842=CARTESIAN_POINT('',(-1.555966115901,0.00138046790836748,5.3559437743963));
#24843=CARTESIAN_POINT('',(-1.55299394346576,0.000305029677950264,5.49405622560371));
#24844=CARTESIAN_POINT('',(-1.5555,-9.09151186476045E-14,-1.2940562256037));
#24845=CARTESIAN_POINT('Ctrl Pts',(-1.555966115901,0.00138046790836748,
5.3559437743963));
#24846=CARTESIAN_POINT('Ctrl Pts',(-1.55217699502656,-0.410255201607083,
5.38545754113982));
#24847=CARTESIAN_POINT('Ctrl Pts',(-1.17320681553292,-1.34462621114732,
5.45200862131617));
#24848=CARTESIAN_POINT('Ctrl Pts',(0.403496653242899,-1.79354886637635,
5.55559701492538));
#24849=CARTESIAN_POINT('Ctrl Pts',(1.72554797232085,-0.634122566945669,
5.66670895522387));
#24850=CARTESIAN_POINT('Ctrl Pts',(1.46886056527041,1.10547479200108,5.77782089552239));
#24851=CARTESIAN_POINT('Ctrl Pts',(-0.131715923640121,1.83365183655613,
5.88893283582089));
#24852=CARTESIAN_POINT('Ctrl Pts',(-1.36662941760285,1.04145067599478,5.9816404621122));
#24853=CARTESIAN_POINT('Ctrl Pts',(-1.55291188141693,0.261131306893961,
6.03731077497067));
#24854=CARTESIAN_POINT('Ctrl Pts',(-1.5529510743802,-2.60258839871949E-5,
6.0559437743963));
#24855=CARTESIAN_POINT('Ctrl Pts',(-1.55299394346576,0.000305029677950229,
5.49405622560371));
#24856=CARTESIAN_POINT('Ctrl Pts',(-1.55250668207154,-0.278154912341265,
5.51392511949124));
#24857=CARTESIAN_POINT('Ctrl Pts',(-1.34792243677793,-1.07688746067556,
5.5708692504912));
#24858=CARTESIAN_POINT('Ctrl Pts',(-0.0687781849042931,-1.83772416168987,
5.66488861860358));
#24859=CARTESIAN_POINT('Ctrl Pts',(1.50750444735784,-1.05327561457109,5.77611432994086));
#24860=CARTESIAN_POINT('Ctrl Pts',(1.70195476716013,0.696642984640571,5.88734004127814));
#24861=CARTESIAN_POINT('Ctrl Pts',(0.336330007005007,1.80799440678846,5.99856575261541));
#24862=CARTESIAN_POINT('Ctrl Pts',(-1.20233240386818,1.30618107352199,6.10080448072394));
#24863=CARTESIAN_POINT('Ctrl Pts',(-1.55176766731418,0.390722855896857,
6.16596797172003));
#24864=CARTESIAN_POINT('Ctrl Pts',(-1.55535150415969,-0.00142776428603842,
6.1940562256037));
#24865=CARTESIAN_POINT('Origin',(0.,0.,-1.2940562256037));
#24866=CARTESIAN_POINT('',(-1.55745403705147,-0.000857197650203868,4.6559437743963));
#24867=CARTESIAN_POINT('',(-1.55647172954169,0.00128913277620515,4.7940562256037));
#24868=CARTESIAN_POINT('',(-1.5555,-9.09151186476045E-14,-1.2940562256037));
#24869=CARTESIAN_POINT('Ctrl Pts',(-1.55745403705147,-0.000857197650203714,
4.6559437743963));
#24870=CARTESIAN_POINT('Ctrl Pts',(-1.55778482013651,-0.0507465481586787,
4.6595296804433));
#24871=CARTESIAN_POINT('Ctrl Pts',(-1.5329809661149,-0.615588902391355,
4.70015289992314));
#24872=CARTESIAN_POINT('Ctrl Pts',(-0.843859631129698,-1.63325682938675,
4.77781343283583));
#24873=CARTESIAN_POINT('Ctrl Pts',(0.914157055608714,-1.59497455450745,
4.88892537313433));
#24874=CARTESIAN_POINT('Ctrl Pts',(1.83579319504673,-0.0974181938582904,
5.00003731343284));
#24875=CARTESIAN_POINT('Ctrl Pts',(1.07782545884778,1.48926801121999,5.11114925373134));
#24876=CARTESIAN_POINT('Ctrl Pts',(-0.666266304296033,1.713393176152,5.22226119402985));
#24877=CARTESIAN_POINT('Ctrl Pts',(-1.49942664147989,0.726761727184559,
5.30385936758484));
#24878=CARTESIAN_POINT('Ctrl Pts',(-1.55693202540547,0.106313199995716,
5.34842022770699));
#24879=CARTESIAN_POINT('Ctrl Pts',(-1.555966115901,0.00138046790836748,
5.3559437743963));
#24880=CARTESIAN_POINT('Ctrl Pts',(-1.55647172954169,0.00128913277620508,
4.7940562256037));
#24881=CARTESIAN_POINT('Ctrl Pts',(-1.55265159250384,-0.427240132487249,
4.82480703015002));
#24882=CARTESIAN_POINT('Ctrl Pts',(-1.14657973682021,-1.37879177584745,
4.89263307180876));
#24883=CARTESIAN_POINT('Ctrl Pts',(0.464983542380115,-1.77925562259896,
4.99753435057992));
#24884=CARTESIAN_POINT('Ctrl Pts',(1.74748619395055,-0.572933012383953,
5.1087600619172));
#24885=CARTESIAN_POINT('Ctrl Pts',(1.42817970701863,1.15856074316792,5.21998577325448));
#24886=CARTESIAN_POINT('Ctrl Pts',(-0.20024807751692,1.82807576816643,5.33121148459175));
#24887=CARTESIAN_POINT('Ctrl Pts',(-1.38701509520349,1.00164745002229,5.4225683020415));
#24888=CARTESIAN_POINT('Ctrl Pts',(-1.55341590891771,0.24144967335499,5.47684988237881));
#24889=CARTESIAN_POINT('Ctrl Pts',(-1.55299394346576,0.000305029677950229,
5.49405622560371));
#24890=CARTESIAN_POINT('Origin',(0.,0.,-1.2940562256037));
#24891=CARTESIAN_POINT('',(-1.55339080467029,-0.000825238370695906,3.9559437743963));
#24892=CARTESIAN_POINT('',(-1.55714699541918,-0.00104284411826,4.0940562256037));
#24893=CARTESIAN_POINT('',(-1.5555,-9.09151186476045E-14,-1.2940562256037));
#24894=CARTESIAN_POINT('Ctrl Pts',(-1.55339080467029,-0.000825238370696021,
3.9559437743963));
#24895=CARTESIAN_POINT('Ctrl Pts',(-1.55438190323133,-0.206647724104582,
3.97063913317962));
#24896=CARTESIAN_POINT('Ctrl Pts',(-1.42057875865067,-0.929976336606789,
4.02237180539578));
#24897=CARTESIAN_POINT('Ctrl Pts',(-0.325039216866852,-1.80941329116195,
4.11114179104478));
#24898=CARTESIAN_POINT('Ctrl Pts',(1.34361459616473,-1.25472178898058,4.22225373134328));
#24899=CARTESIAN_POINT('Ctrl Pts',(1.78296857449566,0.447939743012656,4.3333656716418));
#24900=CARTESIAN_POINT('Ctrl Pts',(0.591048986302979,1.74077225568864,4.44447761194029));
#24901=CARTESIAN_POINT('Ctrl Pts',(-1.08571442614287,1.45061399985919,4.5520036461918));
#24902=CARTESIAN_POINT('Ctrl Pts',(-1.55436830095327,0.464539543423835,
4.62249236701046));
#24903=CARTESIAN_POINT('Ctrl Pts',(-1.55745403705147,-0.000857197650203714,
4.6559437743963));
#24904=CARTESIAN_POINT('Ctrl Pts',(-1.55714699541918,-0.00104284411826003,
4.0940562256037));
#24905=CARTESIAN_POINT('Ctrl Pts',(-1.55763619195644,-0.0644821423710283,
4.09861370369637));
#24906=CARTESIAN_POINT('Ctrl Pts',(-1.52529338404343,-0.643499375005814,
4.14024641890147));
#24907=CARTESIAN_POINT('Ctrl Pts',(-0.799431294618187,-1.65616118233816,
4.21895437121899));
#24908=CARTESIAN_POINT('Ctrl Pts',(0.959104426053338,-1.56910132141185,
4.33018008255627));
#24909=CARTESIAN_POINT('Ctrl Pts',(1.83849028118038,-0.0437463405035559,
4.44140579389354));
#24910=CARTESIAN_POINT('Ctrl Pts',(1.0326493363287,1.52170812080878,4.55263150523082));
#24911=CARTESIAN_POINT('Ctrl Pts',(-0.719755403894915,1.69230978744094,
4.6638572165681));
#24912=CARTESIAN_POINT('Ctrl Pts',(-1.51031879937117,0.693384867678679,
4.74433212335906));
#24913=CARTESIAN_POINT('Ctrl Pts',(-1.55725740651651,0.0894235565985826,
4.78773179303759));
#24914=CARTESIAN_POINT('Ctrl Pts',(-1.55647172954169,0.00128913277620508,
4.7940562256037));
#24915=CARTESIAN_POINT('Origin',(0.,0.,-1.2940562256037));
#24916=CARTESIAN_POINT('',(-1.55444809594431,0.00131769509984214,3.2559437743963));
#24917=CARTESIAN_POINT('',(-1.55323130759427,-0.000686532414708174,3.3940562256037));
#24918=CARTESIAN_POINT('',(-1.5555,-9.09151186476045E-14,-1.2940562256037));
#24919=CARTESIAN_POINT('Ctrl Pts',(-1.55444809594431,0.00131769509984224,
3.2559437743963));
#24920=CARTESIAN_POINT('Ctrl Pts',(-1.55154267442328,-0.359485027434377,
3.28174858591594));
#24921=CARTESIAN_POINT('Ctrl Pts',(-1.24686166172698,-1.24256912580371,
3.34459071086842));
#24922=CARTESIAN_POINT('Ctrl Pts',(0.222653802667342,-1.82484307132901,
3.44447014925373));
#24923=CARTESIAN_POINT('Ctrl Pts',(1.65372145106143,-0.803014516107455,
3.55558208955224));
#24924=CARTESIAN_POINT('Ctrl Pts',(1.57176630825256,0.953508061332994,3.66669402985075));
#24925=CARTESIAN_POINT('Ctrl Pts',(0.0517707715753711,1.83764706567811,
3.77780597014925));
#24926=CARTESIAN_POINT('Ctrl Pts',(-1.30829594910608,1.14591637592306,3.87422255166444));
#24927=CARTESIAN_POINT('Ctrl Pts',(-1.55188399701554,0.312095099942876,
3.93360181974679));
#24928=CARTESIAN_POINT('Ctrl Pts',(-1.55339080467029,-0.000825238370696021,
3.9559437743963));
#24929=CARTESIAN_POINT('Ctrl Pts',(-1.55323130759427,-0.000686532414707983,
3.3940562256037));
#24930=CARTESIAN_POINT('Ctrl Pts',(-1.55409097737417,-0.216984975064148,
3.40949561435515));
#24931=CARTESIAN_POINT('Ctrl Pts',(-1.4109189051218,-0.95160176519996,3.46201024021903));
#24932=CARTESIAN_POINT('Ctrl Pts',(-0.286969261786828,-1.81648256240041,
3.55160010319533));
#24933=CARTESIAN_POINT('Ctrl Pts',(1.37145934362907,-1.22517734450477,3.66282581453261));
#24934=CARTESIAN_POINT('Ctrl Pts',(1.77275862659963,0.489169815626649,3.77405152586988));
#24935=CARTESIAN_POINT('Ctrl Pts',(0.549083125265984,1.75512620009375,3.88527723720716));
#24936=CARTESIAN_POINT('Ctrl Pts',(-1.10713858120128,1.42631885494224,3.99194547045177));
#24937=CARTESIAN_POINT('Ctrl Pts',(-1.5536565617213,0.451598676262059,4.06153846658395));
#24938=CARTESIAN_POINT('Ctrl Pts',(-1.55714699541918,-0.00104284411826003,
4.0940562256037));
#24939=CARTESIAN_POINT('Origin',(0.,0.,-1.2940562256037));
#24940=CARTESIAN_POINT('',(-1.55804749425921,3.19249239839854E-5,2.5559437743963));
#24941=CARTESIAN_POINT('',(-1.55463050379685,0.00136373510819555,2.6940562256037));
#24942=CARTESIAN_POINT('',(-1.5555,-9.09151186476045E-14,-1.2940562256037));
#24943=CARTESIAN_POINT('Ctrl Pts',(-1.55804749425921,3.19249239839832E-5,
2.5559437743963));
#24944=CARTESIAN_POINT('Ctrl Pts',(-1.55789240629065,-0.513022302446059,
2.59285803865226));
#24945=CARTESIAN_POINT('Ctrl Pts',(-1.00056267955874,-1.54112970888597,
2.66680961634105));
#24946=CARTESIAN_POINT('Ctrl Pts',(0.750568915726592,-1.67817557333754,
2.77779850746269));
#24947=CARTESIAN_POINT('Ctrl Pts',(1.81693142975936,-0.279977017554228,
2.8889104477612));
#24948=CARTESIAN_POINT('Ctrl Pts',(1.22094708256035,1.37437810371544,3.0000223880597));
#24949=CARTESIAN_POINT('Ctrl Pts',(-0.492106140687917,1.77128724302598,
3.11113432835821));
#24950=CARTESIAN_POINT('Ctrl Pts',(-1.46164337385231,0.831798954515017,
3.19644145713707));
#24951=CARTESIAN_POINT('Ctrl Pts',(-1.55571278849084,0.158370470628406,
3.2447112724831));
#24952=CARTESIAN_POINT('Ctrl Pts',(-1.55444809594431,0.00131769509984224,
3.2559437743963));
#24953=CARTESIAN_POINT('Ctrl Pts',(-1.55463050379685,0.0013637351081955,
2.6940562256037));
#24954=CARTESIAN_POINT('Ctrl Pts',(-1.55154239698677,-0.366550683268523,
2.72037752501393));
#24955=CARTESIAN_POINT('Ctrl Pts',(-1.23694887232287,-1.2574453593796,2.78377406153659));
#24956=CARTESIAN_POINT('Ctrl Pts',(0.249957593646744,-1.82194441691009,
2.88424583517168));
#24957=CARTESIAN_POINT('Ctrl Pts',(1.6668940398915,-0.776804039943688,2.99547154650895));
#24958=CARTESIAN_POINT('Ctrl Pts',(1.55589501744036,0.980383063583733,3.10669725784622));
#24959=CARTESIAN_POINT('Ctrl Pts',(0.0187062518377651,1.83891553174339,
3.2179229691835));
#24960=CARTESIAN_POINT('Ctrl Pts',(-1.31986995326957,1.12664004660162,3.31370929176933));
#24961=CARTESIAN_POINT('Ctrl Pts',(-1.55202661709144,0.302421341945843,
3.37242037724273));
#24962=CARTESIAN_POINT('Ctrl Pts',(-1.55323130759427,-0.000686532414707983,
3.3940562256037));
#24963=CARTESIAN_POINT('Origin',(0.,0.,-1.2940562256037));
#24964=CARTESIAN_POINT('',(-1.55454086388192,-0.001338238080313,1.8559437743963));
#24965=CARTESIAN_POINT('',(-1.55805913879558,-3.33498767488005E-5,1.9940562256037));
#24966=CARTESIAN_POINT('',(-1.5555,-9.09151186476045E-14,-1.2940562256037));
#24967=CARTESIAN_POINT('Ctrl Pts',(-1.55454086388192,-0.00133823808031298,
1.8559437743963));
#24968=CARTESIAN_POINT('Ctrl Pts',(-1.55580261226994,-0.154926887448841,
1.86693017795574));
#24969=CARTESIAN_POINT('Ctrl Pts',(-1.46434456543453,-0.824823376066396,
1.91495389494802));
#24970=CARTESIAN_POINT('Ctrl Pts',(-0.503833422351614,-1.76798718278107,
2.00001492537314));
#24971=CARTESIAN_POINT('Ctrl Pts',(1.211812440791,-1.38243900779253,2.11112686567164));
#24972=CARTESIAN_POINT('Ctrl Pts',(1.81874690762903,0.2679303086893,2.22223880597015));
#24973=CARTESIAN_POINT('Ctrl Pts',(0.761673489280804,1.67316479305249,2.33335074626865));
#24974=CARTESIAN_POINT('Ctrl Pts',(-0.99227021626331,1.54758740541246,2.44446268656716));
#24975=CARTESIAN_POINT('Ctrl Pts',(-1.5572711215541,0.518216278848874,2.51866036260971));
#24976=CARTESIAN_POINT('Ctrl Pts',(-1.55804801122595,0.00174212832754369,
2.55582072521942));
#24977=CARTESIAN_POINT('Ctrl Pts',(-1.55804749425921,3.19249239839832E-5,
2.5559437743963));
#24978=CARTESIAN_POINT('Ctrl Pts',(-1.55805913879558,-3.33498767486382E-5,
1.9940562256037));
#24979=CARTESIAN_POINT('Ctrl Pts',(-1.5580596990309,-0.00181195213168648,
1.99418419856029));
#24980=CARTESIAN_POINT('Ctrl Pts',(-1.5572509939767,-0.518871555499298,
2.0313874086293));
#24981=CARTESIAN_POINT('Ctrl Pts',(-0.990825815880477,-1.5492657736205,
2.10566585581074));
#24982=CARTESIAN_POINT('Ctrl Pts',(0.765574959497512,-1.6720811124538,2.21689156714802));
#24983=CARTESIAN_POINT('Ctrl Pts',(1.82022199392772,-0.262206313316451,
2.32811727848529));
#24984=CARTESIAN_POINT('Ctrl Pts',(1.20638759997596,1.38801628675575,2.43934298982257));
#24985=CARTESIAN_POINT('Ctrl Pts',(-0.513265374585843,1.76593287340023,
2.55056870115984));
#24986=CARTESIAN_POINT('Ctrl Pts',(-1.46682634638563,0.818764115677731,
2.63547311308689));
#24987=CARTESIAN_POINT('Ctrl Pts',(-1.55589219334096,0.151680354105525,
2.68330228790151));
#24988=CARTESIAN_POINT('Ctrl Pts',(-1.55463050379685,0.0013637351081955,
2.6940562256037));
#24989=CARTESIAN_POINT('Origin',(0.,0.,-1.2940562256037));
#24990=CARTESIAN_POINT('',(-1.55333683422467,0.00078011305757314,1.1559437743963));
#24991=CARTESIAN_POINT('',(-1.55453190133567,-0.00134444967022529,1.2940562256037));
#24992=CARTESIAN_POINT('',(-1.5555,-9.09151186476045E-14,-1.2940562256037));
#24993=CARTESIAN_POINT('Ctrl Pts',(-1.55333683422467,0.000780113057573043,
1.1559437743963));
#24994=CARTESIAN_POINT('Ctrl Pts',(-1.55193443781686,-0.308720927367064,
1.17803963069206));
#24995=CARTESIAN_POINT('Ctrl Pts',(-1.31240187276934,-1.13901289380036,
1.23717280042066));
#24996=CARTESIAN_POINT('Ctrl Pts',(0.0395921340189295,-1.83794780075079,
1.33334328358209));
#24997=CARTESIAN_POINT('Ctrl Pts',(1.56541283438613,-0.96390406493211,1.44445522388059));
#24998=CARTESIAN_POINT('Ctrl Pts',(1.65900671048959,0.792038431388639,1.55556716417911));
#24999=CARTESIAN_POINT('Ctrl Pts',(0.234741865039883,1.82332721494359,1.66667910447761));
#25000=CARTESIAN_POINT('Ctrl Pts',(-1.24223016373737,1.24939407250205,1.76680464121668));
#25001=CARTESIAN_POINT('Ctrl Pts',(-1.55154901187489,0.362850464858491,
1.8298928645229));
#25002=CARTESIAN_POINT('Ctrl Pts',(-1.55454086388192,-0.00133823808031298,
1.8559437743963));
#25003=CARTESIAN_POINT('Ctrl Pts',(-1.55453190133567,-0.00134444967022513,
1.2940562256037));
#25004=CARTESIAN_POINT('Ctrl Pts',(-1.55579946924303,-0.155263418355649,
1.30506610921907));
#25005=CARTESIAN_POINT('Ctrl Pts',(-1.46404280977096,-0.826019057429759,
1.35315122994686));
#25006=CARTESIAN_POINT('Ctrl Pts',(-0.501082205369057,-1.76942810040879,
1.43831158778708));
#25007=CARTESIAN_POINT('Ctrl Pts',(1.21592516185098,-1.37966899434435,1.54953729912436));
#25008=CARTESIAN_POINT('Ctrl Pts',(1.8183716526183,0.274745208061178,1.66076301046163));
#25009=CARTESIAN_POINT('Ctrl Pts',(0.754032712405612,1.67731773070425,1.77198872179891));
#25010=CARTESIAN_POINT('Ctrl Pts',(-0.999460041113845,1.5425554247787,1.8830864601796));
#25011=CARTESIAN_POINT('Ctrl Pts',(-1.5578973924169,0.513469573665662,1.95710896144786));
#25012=CARTESIAN_POINT('Ctrl Pts',(-1.55805913879558,-3.33498767486382E-5,
1.9940562256037));
#25013=CARTESIAN_POINT('Origin',(0.,0.,-1.2940562256037));
#25014=CARTESIAN_POINT('',(-1.55735958542387,0.00101297198046619,0.455943774396298));
#25015=CARTESIAN_POINT('',(-1.55327638232574,0.000749985450956003,0.594056225603703));
#25016=CARTESIAN_POINT('',(-1.5555,-9.09151186476045E-14,-1.2940562256037));
#25017=CARTESIAN_POINT('Ctrl Pts',(-1.55735958542387,0.00101297198046621,
0.455943774396298));
#25018=CARTESIAN_POINT('Ctrl Pts',(-1.55415428451722,-0.460990851268869,
0.489149083428377));
#25019=CARTESIAN_POINT('Ctrl Pts',(-1.09150079880486,-1.44424863810505,
0.559391705893293));
#25020=CARTESIAN_POINT('Ctrl Pts',(0.579516952736672,-1.74455562530747,
0.666671641791043));
#25021=CARTESIAN_POINT('Ctrl Pts',(1.77995215483547,-0.45979539180552,0.777783582089551));
#25022=CARTESIAN_POINT('Ctrl Pts',(1.35190460952174,1.24581651128198,0.888895522388059));
#25023=CARTESIAN_POINT('Ctrl Pts',(-0.313043761712607,1.81151378121076,
1.00000746268657));
#25024=CARTESIAN_POINT('Ctrl Pts',(-1.41743746237044,0.936955068058493,
1.08902354668931));
#25025=CARTESIAN_POINT('Ctrl Pts',(-1.55428514985164,0.21006806585223,1.14100231725922));
#25026=CARTESIAN_POINT('Ctrl Pts',(-1.55333683422467,0.000780113057573043,
1.1559437743963));
#25027=CARTESIAN_POINT('Ctrl Pts',(-1.55327638232574,0.000749985450955847,
0.594056225603703));
#25028=CARTESIAN_POINT('Ctrl Pts',(-1.55196556188379,-0.305924499715954,
0.61594801987785));
#25029=CARTESIAN_POINT('Ctrl Pts',(-1.3156705723219,-1.13385132195631,0.674915051264423));
#25030=CARTESIAN_POINT('Ctrl Pts',(0.0313843551128396,-1.83872969125081,
0.770957319763422));
#25031=CARTESIAN_POINT('Ctrl Pts',(1.56261245507102,-0.969643437172017,
0.882183031100698));
#25032=CARTESIAN_POINT('Ctrl Pts',(1.66150197094076,0.788277540412492,0.993408742437974));
#25033=CARTESIAN_POINT('Ctrl Pts',(0.237394066880885,1.82362194812979,1.10463445377525));
#25034=CARTESIAN_POINT('Ctrl Pts',(-1.24180780125352,1.25035520807598,1.20485028149716));
#25035=CARTESIAN_POINT('Ctrl Pts',(-1.55153099717163,0.363051076099792,
1.26799087210664));
#25036=CARTESIAN_POINT('Ctrl Pts',(-1.55453190133567,-0.00134444967022513,
1.2940562256037));
#25037=CARTESIAN_POINT('Origin',(0.,0.,7.5));
#25038=CARTESIAN_POINT('',(-1.90714972453263,0.000559583190138325,7.09553262944276));
#25039=CARTESIAN_POINT('Ctrl Pts',(-0.352169241380463,1.51510959188618,
7.4445));
#25040=CARTESIAN_POINT('Ctrl Pts',(-0.294581668876612,1.53128067531421,
7.44178679402676));
#25041=CARTESIAN_POINT('Ctrl Pts',(-0.236177221040451,1.54382025621514,
7.43908623010619));
#25042=CARTESIAN_POINT('Ctrl Pts',(-0.17725379571509,1.55288079770358,7.43639376053775));
#25043=CARTESIAN_POINT('Ctrl Pts',(-0.119240420394871,1.56180140255761,
7.43374287514286));
#25044=CARTESIAN_POINT('Ctrl Pts',(-0.0607231436400752,1.56734934022223,
7.4310998360025));
#25045=CARTESIAN_POINT('Ctrl Pts',(-0.00197185718845893,1.56962582506071,
7.42846030289105));
#25046=CARTESIAN_POINT('Ctrl Pts',(0.0296117181373077,1.57084962005681,
7.4270413400413));
#25047=CARTESIAN_POINT('Ctrl Pts',(0.0612630953454002,1.57112724793077,
7.42562339041052));
#25048=CARTESIAN_POINT('Ctrl Pts',(0.0929408476792332,1.57046939552494,
7.42420577971289));
#25049=CARTESIAN_POINT('Ctrl Pts',(0.105200379607973,1.57021480162293,7.42365715355322));
#25050=CARTESIAN_POINT('Ctrl Pts',(0.117460267523568,1.56982005993498,7.42310873898429));
#25051=CARTESIAN_POINT('Ctrl Pts',(0.129708286104984,1.56928654809906,7.42256093565192));
#25052=CARTESIAN_POINT('Ctrl Pts',(0.192428535028528,1.56655451475585,7.41975571771902));
#25053=CARTESIAN_POINT('Ctrl Pts',(0.254912080108278,1.56018641116159,7.41696316059146));
#25054=CARTESIAN_POINT('Ctrl Pts',(0.316835955987319,1.55031158486179,7.41417821827426));
#25055=CARTESIAN_POINT('Ctrl Pts',(0.379261168612821,1.54035681180124,7.41137072901695));
#25056=CARTESIAN_POINT('Ctrl Pts',(0.441118681165113,1.52683817797346,7.40857097836836));
#25057=CARTESIAN_POINT('Ctrl Pts',(0.502077268456636,1.50983552777742,7.40577379678119));
#25058=CARTESIAN_POINT('Ctrl Pts',(0.518104654250298,1.50536514802758,7.40503835473071));
#25059=CARTESIAN_POINT('Ctrl Pts',(0.534069848209942,1.50065364953946,7.40430309027496));
#25060=CARTESIAN_POINT('Ctrl Pts',(0.549966680795085,1.49570190223715,7.40356790945547));
#25061=CARTESIAN_POINT('Ctrl Pts',(0.559908491182372,1.4926051008774,7.40310813054867));
#25062=CARTESIAN_POINT('Ctrl Pts',(0.569821116728089,1.48941503409471,7.4026484967243));
#25063=CARTESIAN_POINT('Ctrl Pts',(0.579694961183896,1.486134869268,7.40218936420725));
#25064=CARTESIAN_POINT('Ctrl Pts',(0.640449229714658,1.46595184779153,7.39936429841276));
#25065=CARTESIAN_POINT('Ctrl Pts',(0.69982505895545,1.44233435228215,7.39655407027566));
#25066=CARTESIAN_POINT('Ctrl Pts',(0.757493396577592,1.41540064986381,7.39375356846506));
#25067=CARTESIAN_POINT('Ctrl Pts',(0.814802366573082,1.38863478825924,7.39097051833992));
#25068=CARTESIAN_POINT('Ctrl Pts',(0.870426121162267,1.35859365369072,7.38819707369729));
#25069=CARTESIAN_POINT('Ctrl Pts',(0.924030095744784,1.32534364884642,7.38542821816778));
#25070=CARTESIAN_POINT('Ctrl Pts',(0.960999915716867,1.30241164235365,7.38351858196539));
#25071=CARTESIAN_POINT('Ctrl Pts',(0.997008764456124,1.27795226352036,7.38161112864094));
#25072=CARTESIAN_POINT('Ctrl Pts',(1.03193962221215,1.25197434532887,7.3797042125328));
#25073=CARTESIAN_POINT('Ctrl Pts',(1.0531065792895,1.23623257674251,7.37854868375383));
#25074=CARTESIAN_POINT('Ctrl Pts',(1.07387756970412,1.21993300461795,7.37739335223873));
#25075=CARTESIAN_POINT('Ctrl Pts',(1.09422502955045,1.2030757852037,7.37623785181303));
#25076=CARTESIAN_POINT('Ctrl Pts',(1.10258166584356,1.19615257942657,7.37576329150589));
#25077=CARTESIAN_POINT('Ctrl Pts',(1.11086633597203,1.18913559341204,7.3752887282991));
#25078=CARTESIAN_POINT('Ctrl Pts',(1.11906690491304,1.18203401934788,7.37481473623418));
#25079=CARTESIAN_POINT('Ctrl Pts',(1.12385025457867,1.17789170773882,7.37453825910173));
#25080=CARTESIAN_POINT('Ctrl Pts',(1.12860592464056,1.17371985114455,7.37426192347451));
#25081=CARTESIAN_POINT('Ctrl Pts',(1.13333360310225,1.16951854601392,7.37398572456616));
#25082=CARTESIAN_POINT('Ctrl Pts',(1.17895537492945,1.12897624060986,7.37132042410681));
#25083=CARTESIAN_POINT('Ctrl Pts',(1.22197272212526,1.08569548753383,7.36866785506909));
#25084=CARTESIAN_POINT('Ctrl Pts',(1.2623504524016,1.0400250384405,7.36602371637222));
#25085=CARTESIAN_POINT('Ctrl Pts',(1.30450707484485,0.992342519733652,7.36326308678831));
#25086=CARTESIAN_POINT('Ctrl Pts',(1.34378698003833,0.942054513171778,7.36051164672689));
#25087=CARTESIAN_POINT('Ctrl Pts',(1.38011608577908,0.889512321374444,7.35776450122604));
#25088=CARTESIAN_POINT('Ctrl Pts',(1.41047885103542,0.845599150293909,7.35546852029652));
#25089=CARTESIAN_POINT('Ctrl Pts',(1.43877996472123,0.800110306074669,7.35317553916464));
#25090=CARTESIAN_POINT('Ctrl Pts',(1.46495451960825,0.753233209535809,7.35088270017959));
#25091=CARTESIAN_POINT('Ctrl Pts',(1.47224608288955,0.740174446270043,7.35024397372845));
#25092=CARTESIAN_POINT('Ctrl Pts',(1.47937249019278,0.727007875170104,7.34960525830843));
#25093=CARTESIAN_POINT('Ctrl Pts',(1.48633203561836,0.713737394565328,7.34896649214163));
#25094=CARTESIAN_POINT('Ctrl Pts',(1.49231636613785,0.702326456460141,7.34841723387359));
#25095=CARTESIAN_POINT('Ctrl Pts',(1.49817791288619,0.690837217360077,7.34786787112171));
#25096=CARTESIAN_POINT('Ctrl Pts',(1.50390644072503,0.679291229674037,7.3473192635151));
#25097=CARTESIAN_POINT('Ctrl Pts',(1.53283760232342,0.620979767295612,7.34454859437159));
#25098=CARTESIAN_POINT('Ctrl Pts',(1.55843652026989,0.561117048195595,7.34179201389979));
#25099=CARTESIAN_POINT('Ctrl Pts',(1.58063784893836,0.500065381838401,7.33904470742869));
#25100=CARTESIAN_POINT('Ctrl Pts',(1.6031119912636,0.438263502347606,7.3362636415941));
#25101=CARTESIAN_POINT('Ctrl Pts',(1.62210502961578,0.375242296860671,7.33349207908152));
#25102=CARTESIAN_POINT('Ctrl Pts',(1.63750518239391,0.311348169568812,7.33072502553951));
#25103=CARTESIAN_POINT('Ctrl Pts',(1.65022992907376,0.258554109936303,7.32843868098962));
#25104=CARTESIAN_POINT('Ctrl Pts',(1.66050103147123,0.20516326683894,7.32615541484386));
#25105=CARTESIAN_POINT('Ctrl Pts',(1.66822949082188,0.151363515297575,7.32387240968315));
#25106=CARTESIAN_POINT('Ctrl Pts',(1.67108031331177,0.13151822211743,7.32303026998087));
#25107=CARTESIAN_POINT('Ctrl Pts',(1.67358492004799,0.111617257557933,7.32218816579018));
#25108=CARTESIAN_POINT('Ctrl Pts',(1.67573795844748,0.091670001678837,7.32134595570008));
#25109=CARTESIAN_POINT('Ctrl Pts',(1.67695445834914,0.0803994944639542,
7.32087009400991));
#25110=CARTESIAN_POINT('Ctrl Pts',(1.67805865914088,0.0691137533863127,
7.3203941797156));
#25111=CARTESIAN_POINT('Ctrl Pts',(1.67904845798992,0.0578298683786967,
7.31991883455417));
#25112=CARTESIAN_POINT('Ctrl Pts',(1.68482856592515,-0.00806440229655341,
7.31714297121365));
#25113=CARTESIAN_POINT('Ctrl Pts',(1.68672581172374,-0.0740201346390124,
7.31438118276366));
#25114=CARTESIAN_POINT('Ctrl Pts',(1.68463949062778,-0.139690992105407,
7.31162863136205));
#25115=CARTESIAN_POINT('Ctrl Pts',(1.68257287237932,-0.204741665606402,
7.30890207456915));
#25116=CARTESIAN_POINT('Ctrl Pts',(1.67659788793627,-0.2695138491763,7.30618458118234));
#25117=CARTESIAN_POINT('Ctrl Pts',(1.6665669476348,-0.3336793478161,7.30347144913232));
#25118=CARTESIAN_POINT('Ctrl Pts',(1.65656393293128,-0.397666213161047,
7.30076587029591));
#25119=CARTESIAN_POINT('Ctrl Pts',(1.64252742158424,-0.461050667219861,
7.29806462854663));
#25120=CARTESIAN_POINT('Ctrl Pts',(1.62468485220914,-0.523589263699737,
7.29536306097687));
#25121=CARTESIAN_POINT('Ctrl Pts',(1.62063291677799,-0.537791386138751,
7.29474955195105));
#25122=CARTESIAN_POINT('Ctrl Pts',(1.61638449230085,-0.551949831001097,
7.29413602612215));
#25123=CARTESIAN_POINT('Ctrl Pts',(1.61194189299792,-0.566061632343824,
7.29352242888019));
#25124=CARTESIAN_POINT('Ctrl Pts',(1.60819661792182,-0.577958401384625,
7.29300514377289));
#25125=CARTESIAN_POINT('Ctrl Pts',(1.60431575784587,-0.589814146380397,
7.2924881495291));
#25126=CARTESIAN_POINT('Ctrl Pts',(1.60030378247776,-0.601620053553602,
7.29197172819479));
#25127=CARTESIAN_POINT('Ctrl Pts',(1.57922949506156,-0.663634661857349,
7.28925904662807));
#25128=CARTESIAN_POINT('Ctrl Pts',(1.55452233752644,-0.724336859414935,
7.28655946062951));
#25129=CARTESIAN_POINT('Ctrl Pts',(1.52646885207918,-0.783492431203164,
7.28386844992972));
#25130=CARTESIAN_POINT('Ctrl Pts',(1.49785765329009,-0.843824036953083,
7.28112394097306));
#25131=CARTESIAN_POINT('Ctrl Pts',(1.46576530908513,-0.902547787676455,
7.27838835166439));
#25132=CARTESIAN_POINT('Ctrl Pts',(1.43044176155356,-0.95940342094092,7.27565688674544));
#25133=CARTESIAN_POINT('Ctrl Pts',(1.40719192683218,-0.996825598744453,
7.27385904614475));
#25134=CARTESIAN_POINT('Ctrl Pts',(1.38254116404519,-1.03343820105651,7.27206299232293));
#25135=CARTESIAN_POINT('Ctrl Pts',(1.35654982896749,-1.06916144614065,7.2702673579332));
#25136=CARTESIAN_POINT('Ctrl Pts',(1.34005703462379,-1.09182962123443,7.26912793863759));
#25137=CARTESIAN_POINT('Ctrl Pts',(1.32302428798857,-1.11413959500617,7.26798868822771));
#25138=CARTESIAN_POINT('Ctrl Pts',(1.30546545072429,-1.13606969941564,7.26684925734159));
#25139=CARTESIAN_POINT('Ctrl Pts',(1.29557863985671,-1.1484178288128,7.26620768082384));
#25140=CARTESIAN_POINT('Ctrl Pts',(1.28552143085819,-1.16064953781435,7.26556582874875));
#25141=CARTESIAN_POINT('Ctrl Pts',(1.27531693894013,-1.17273679271259,7.26492492457875));
#25142=CARTESIAN_POINT('Ctrl Pts',(1.23124484751569,-1.2249403328029,7.26215692913113));
#25143=CARTESIAN_POINT('Ctrl Pts',(1.18437118678711,-1.27452793646465,7.25940270292496));
#25144=CARTESIAN_POINT('Ctrl Pts',(1.1349613540182,-1.32123869434595,7.25665745327404));
#25145=CARTESIAN_POINT('Ctrl Pts',(1.0857776821155,-1.36773564568569,7.25392476930092));
#25146=CARTESIAN_POINT('Ctrl Pts',(1.03408031096501,-1.41138288844598,7.25120097989535));
#25147=CARTESIAN_POINT('Ctrl Pts',(0.980088635865932,-1.45189422149834,
7.24848135788222));
#25148=CARTESIAN_POINT('Ctrl Pts',(0.928612197667789,-1.49051830805181,
7.24588843120928));
#25149=CARTESIAN_POINT('Ctrl Pts',(0.875049469874555,-1.52629233307795,
7.24329929269164));
#25150=CARTESIAN_POINT('Ctrl Pts',(0.819562927233232,-1.55893273310611,
7.24070984551053));
#25151=CARTESIAN_POINT('Ctrl Pts',(0.806531597661789,-1.56659851637287,
7.24010169913812));
#25152=CARTESIAN_POINT('Ctrl Pts',(0.793394057897985,-1.57409127964972,
7.2394935357407));
#25153=CARTESIAN_POINT('Ctrl Pts',(0.78015224431478,-1.58140700410033,7.23888530224817));
#25154=CARTESIAN_POINT('Ctrl Pts',(0.770009447983695,-1.58701060987914,
7.23841941527599));
#25155=CARTESIAN_POINT('Ctrl Pts',(0.759805087672894,-1.59251043302504,
7.23795347189941));
#25156=CARTESIAN_POINT('Ctrl Pts',(0.749553755678445,-1.59789772385032,
7.23748806565584));
#25157=CARTESIAN_POINT('Ctrl Pts',(0.716202490399591,-1.61542451603163,
7.23597393197059));
#25158=CARTESIAN_POINT('Ctrl Pts',(0.682319909404191,-1.63177984026051,
7.23446389597977));
#25159=CARTESIAN_POINT('Ctrl Pts',(0.647945625107734,-1.64691812240344,
7.23295717369848));
#25160=CARTESIAN_POINT('Ctrl Pts',(0.587919642023283,-1.67335329876966,
7.23032606477447));
#25161=CARTESIAN_POINT('Ctrl Pts',(0.52639576498612,-1.69608014520221,7.22770506060276));
#25162=CARTESIAN_POINT('Ctrl Pts',(0.46370862765048,-1.71520377795159,7.22508998649035));
#25163=CARTESIAN_POINT('Ctrl Pts',(0.400150801058184,-1.73459302725791,
7.22243859046197));
#25164=CARTESIAN_POINT('Ctrl Pts',(0.335396320744255,-1.75027834108098,
7.21979329036732));
#25165=CARTESIAN_POINT('Ctrl Pts',(0.269772608446838,-1.76232212244813,
7.21714973513363));
#25166=CARTESIAN_POINT('Ctrl Pts',(0.241062234316718,-1.76759127679625,
7.2159931797189));
#25167=CARTESIAN_POINT('Ctrl Pts',(0.2121852884367,-1.77216281037181,7.21483695828146));
#25168=CARTESIAN_POINT('Ctrl Pts',(0.183168585619119,-1.77603911617646,
7.21368070646147));
#25169=CARTESIAN_POINT('Ctrl Pts',(0.164433789661126,-1.77854187463173,
7.21293416602716));
#25170=CARTESIAN_POINT('Ctrl Pts',(0.145640727943501,-1.78075477785065,
7.21218761292724));
#25171=CARTESIAN_POINT('Ctrl Pts',(0.126796600025785,-1.78267808932064,
7.21144094909238));
#25172=CARTESIAN_POINT('Ctrl Pts',(0.114847127630937,-1.78389770306013,
7.21096747327424));
#25173=CARTESIAN_POINT('Ctrl Pts',(0.102876237812544,-1.78500084411828,
7.21049391856396));
#25174=CARTESIAN_POINT('Ctrl Pts',(0.0909023739078884,-1.78598642534176,
7.21002091434047));
#25175=CARTESIAN_POINT('Ctrl Pts',(0.0223150311249881,-1.79163192104421,
7.20731150465678));
#25176=CARTESIAN_POINT('Ctrl Pts',(-0.0464949765975819,-1.79343822563924,
7.204615131498));
#25177=CARTESIAN_POINT('Ctrl Pts',(-0.115169948787061,-1.79150548386327,
7.201927305065));
#25178=CARTESIAN_POINT('Ctrl Pts',(-0.184810802193317,-1.78954555898233,
7.1992016756161));
#25179=CARTESIAN_POINT('Ctrl Pts',(-0.254313838210283,-1.78374072590431,
7.19648483499498));
#25180=CARTESIAN_POINT('Ctrl Pts',(-0.323317077031426,-1.77414310096439,
7.19377210128489));
#25181=CARTESIAN_POINT('Ctrl Pts',(-0.390207228852162,-1.76483938420678,
7.19114243965136));
#25182=CARTESIAN_POINT('Ctrl Pts',(-0.456628689115353,-1.75197132856033,
7.18851663724823));
#25183=CARTESIAN_POINT('Ctrl Pts',(-0.522247153731527,-1.73553989954365,
7.18589042924469));
#25184=CARTESIAN_POINT('Ctrl Pts',(-0.542667798244601,-1.73042639417967,
7.18507314617701));
#25185=CARTESIAN_POINT('Ctrl Pts',(-0.563010584939934,-1.72496745463069,
7.1842558238281));
#25186=CARTESIAN_POINT('Ctrl Pts',(-0.583265123016525,-1.71916221233715,
7.18343833365983));
#25187=CARTESIAN_POINT('Ctrl Pts',(-0.594324986363522,-1.71599229623144,
7.18299194828612));
#25188=CARTESIAN_POINT('Ctrl Pts',(-0.605348577565269,-1.71272196767285,
7.18254591460309));
#25189=CARTESIAN_POINT('Ctrl Pts',(-0.616333858846904,-1.70935174383982,
7.18210023125036));
#25190=CARTESIAN_POINT('Ctrl Pts',(-0.683725730938223,-1.68867628841438,
7.17936607863924));
#25191=CARTESIAN_POINT('Ctrl Pts',(-0.749681756569652,-1.66424383897131,
7.17664487770965));
#25192=CARTESIAN_POINT('Ctrl Pts',(-0.813838416597903,-1.63611281928401,
7.17393200937892));
#25193=CARTESIAN_POINT('Ctrl Pts',(-0.876849560193779,-1.60848407863208,
7.17126757928126));
#25194=CARTESIAN_POINT('Ctrl Pts',(-0.938126029319885,-1.57728744952324,
7.16861118688198));
#25195=CARTESIAN_POINT('Ctrl Pts',(-0.997312296090875,-1.54253001527406,
7.16595845612799));
#25196=CARTESIAN_POINT('Ctrl Pts',(-1.02347117496609,-1.52716808146505,
7.16478601417029));
#25197=CARTESIAN_POINT('Ctrl Pts',(-1.0492215115725,-1.51110995120918,7.16361428748691));
#25198=CARTESIAN_POINT('Ctrl Pts',(-1.07453112510484,-1.49435330423123,
7.16244289826465));
#25199=CARTESIAN_POINT('Ctrl Pts',(-1.10516814559263,-1.47406955963299,
7.16102494395429));
#25200=CARTESIAN_POINT('Ctrl Pts',(-1.13515946112038,-1.45276234916859,
7.15960748412057));
#25201=CARTESIAN_POINT('Ctrl Pts',(-1.16448435570839,-1.43047866030764,
7.15818984863178));
#25202=CARTESIAN_POINT('Ctrl Pts',(-1.17968931872586,-1.41892456370188,
7.15745480438074));
#25203=CARTESIAN_POINT('Ctrl Pts',(-1.1947150759586,-1.40710789339051,7.15671971290617));
#25204=CARTESIAN_POINT('Ctrl Pts',(-1.20955844125675,-1.39503487170675,
7.15598448079515));
#25205=CARTESIAN_POINT('Ctrl Pts',(-1.2184705964626,-1.38778606788849,7.1555430375945));
#25206=CARTESIAN_POINT('Ctrl Pts',(-1.22730979594949,-1.38045068721632,
7.15510189992037));
#25207=CARTESIAN_POINT('Ctrl Pts',(-1.23607420347025,-1.37303174210186,
7.15466112096385));
#25208=CARTESIAN_POINT('Ctrl Pts',(-1.28876418024182,-1.32843043336258,
7.1520112404185));
#25209=CARTESIAN_POINT('Ctrl Pts',(-1.33877042848354,-1.2807988909053,7.14937346465996));
#25210=CARTESIAN_POINT('Ctrl Pts',(-1.38599825103533,-1.23050256527184,
7.14674359103655));
#25211=CARTESIAN_POINT('Ctrl Pts',(-1.43425343070737,-1.17911213270163,
7.14405650919887));
#25212=CARTESIAN_POINT('Ctrl Pts',(-1.47960859192691,-1.1249390060584,7.14137767702936));
#25213=CARTESIAN_POINT('Ctrl Pts',(-1.52193138288134,-1.06832685423381,
7.13870261160338));
#25214=CARTESIAN_POINT('Ctrl Pts',(-1.55066539724144,-1.02989143098312,
7.13688644195504));
#25215=CARTESIAN_POINT('Ctrl Pts',(-1.57800101601077,-0.990330805152557,
7.13507200854792));
#25216=CARTESIAN_POINT('Ctrl Pts',(-1.60388667803358,-0.949743456777433,
7.13325790847962));
#25217=CARTESIAN_POINT('Ctrl Pts',(-1.62003594041973,-0.924422267854757,
7.13212614766269));
#25218=CARTESIAN_POINT('Ctrl Pts',(-1.63562069179463,-0.898701332888775,
7.13099451658541));
#25219=CARTESIAN_POINT('Ctrl Pts',(-1.65062655993749,-0.872603512387977,
7.12986267459833));
#25220=CARTESIAN_POINT('Ctrl Pts',(-1.65635574489922,-0.862639461036616,
7.12943054151348));
#25221=CARTESIAN_POINT('Ctrl Pts',(-1.66200053139848,-0.852620464599865,
7.12899837768465));
#25222=CARTESIAN_POINT('Ctrl Pts',(-1.66756006049801,-0.842547771324513,
7.12856616415337));
#25223=CARTESIAN_POINT('Ctrl Pts',(-1.67344140782474,-0.831892011347815,
7.12810893156204));
#25224=CARTESIAN_POINT('Ctrl Pts',(-1.67922337730384,-0.821183277061747,
7.1276519494335));
#25225=CARTESIAN_POINT('Ctrl Pts',(-1.68490302697532,-0.810427767612281,
7.1271953846437));
#25226=CARTESIAN_POINT('Ctrl Pts',(-1.71867201689079,-0.746479687863883,
7.12448082781816));
#25227=CARTESIAN_POINT('Ctrl Pts',(-1.74885449180758,-0.680831600304512,
7.12177889893296));
#25228=CARTESIAN_POINT('Ctrl Pts',(-1.77532011389704,-0.613841133314895,
7.11908508207449));
#25229=CARTESIAN_POINT('Ctrl Pts',(-1.80172135822353,-0.547013620983615,
7.11639781793949));
#25230=CARTESIAN_POINT('Ctrl Pts',(-1.82442431805884,-0.478849290745972,
7.11371862641413));
#25231=CARTESIAN_POINT('Ctrl Pts',(-1.84325651205081,-0.409674689769748,
7.11104302445964));
#25232=CARTESIAN_POINT('Ctrl Pts',(-1.86148527154818,-0.34271663033918,
7.10845315603751));
#25233=CARTESIAN_POINT('Ctrl Pts',(-1.87608759212419,-0.274811091848995,
7.10586665083265));
#25234=CARTESIAN_POINT('Ctrl Pts',(-1.88686151657838,-0.206241373327113,
7.1032794430912));
#25235=CARTESIAN_POINT('Ctrl Pts',(-1.8894237591873,-0.189934199908044,
7.10266415625292));
#25236=CARTESIAN_POINT('Ctrl Pts',(-1.89176925852511,-0.173589436851263,
7.10204882968071));
#25237=CARTESIAN_POINT('Ctrl Pts',(-1.89389487850133,-0.157210868172391,
7.10143340868806));
#25238=CARTESIAN_POINT('Ctrl Pts',(-1.89540717923759,-0.145558116622667,
7.10099555919912));
#25239=CARTESIAN_POINT('Ctrl Pts',(-1.89680805540638,-0.133888495556873,
7.10055767143479));
#25240=CARTESIAN_POINT('Ctrl Pts',(-1.89809506960791,-0.12221735851089,
7.10012024866215));
#25241=CARTESIAN_POINT('Ctrl Pts',(-1.90260558085945,-0.0813143172688235,
7.09858724278285));
#25242=CARTESIAN_POINT('Ctrl Pts',(-1.90572389008592,-0.0403491830271802,
7.09705830708501));
#25243=CARTESIAN_POINT('Ctrl Pts',(-1.90742224034152,0.000616434489977578,
7.09553262952215));
#25244=CARTESIAN_POINT('',(0.084982434829279,1.94905960819019,7.046));
#25245=CARTESIAN_POINT('Ctrl Pts',(0.0849160311153282,1.94854955259671,
7.046));
#25246=CARTESIAN_POINT('Ctrl Pts',(0.0133469932817959,1.94202022424704,
7.05556311378236));
#25247=CARTESIAN_POINT('Ctrl Pts',(-0.057643443386169,1.9317481562341,7.06516697216295));
#25248=CARTESIAN_POINT('Ctrl Pts',(-0.127716536696194,1.91775362299336,
7.07483035053949));
#25249=CARTESIAN_POINT('Ctrl Pts',(-0.195999508457667,1.90411660095032,
7.08424686352096));
#25250=CARTESIAN_POINT('Ctrl Pts',(-0.263412231749455,1.88694439734026,
7.09371989428859));
#25251=CARTESIAN_POINT('Ctrl Pts',(-0.329616946053496,1.86621372408347,
7.10326681575032));
#25252=CARTESIAN_POINT('Ctrl Pts',(-0.373950818831073,1.85233146448275,
7.10965989524551));
#25253=CARTESIAN_POINT('Ctrl Pts',(-0.41774246810674,1.83685263442241,7.11608610945697));
#25254=CARTESIAN_POINT('Ctrl Pts',(-0.460881457798893,1.81976080684648,
7.12255067528795));
#25255=CARTESIAN_POINT('Ctrl Pts',(-0.497884301533585,1.80510014303758,
7.12809571287374));
#25256=CARTESIAN_POINT('Ctrl Pts',(-0.53440686918178,1.7892525808674,7.13366896766314));
#25257=CARTESIAN_POINT('Ctrl Pts',(-0.570374125039445,1.77220369526276,
7.13927373202269));
#25258=CARTESIAN_POINT('Ctrl Pts',(-0.580625413497348,1.76734446872319,
7.14087118656344));
#25259=CARTESIAN_POINT('Ctrl Pts',(-0.590829427779041,1.7623885644236,7.14247087519816));
#25260=CARTESIAN_POINT('Ctrl Pts',(-0.600974912742468,1.75734066833771,
7.14407135449713));
#25261=CARTESIAN_POINT('Ctrl Pts',(-0.660532286239387,1.72770783820246,
7.15346670067592));
#25262=CARTESIAN_POINT('Ctrl Pts',(-0.718171394717493,1.69486290257124,
7.16290421661148));
#25263=CARTESIAN_POINT('Ctrl Pts',(-0.77359140837187,1.65879255638639,7.17240215454285));
#25264=CARTESIAN_POINT('Ctrl Pts',(-0.79145555504589,1.64716560228914,7.17546373004814));
#25265=CARTESIAN_POINT('Ctrl Pts',(-0.809088855973432,1.63520322368412,
7.17853158362642));
#25266=CARTESIAN_POINT('Ctrl Pts',(-0.826480388876073,1.62290416848565,
7.18160632658995));
#25267=CARTESIAN_POINT('Ctrl Pts',(-0.88415727734301,1.5821158585131,7.19180333498275));
#25268=CARTESIAN_POINT('Ctrl Pts',(-0.93917932864386,1.5376265413157,7.20207611531283));
#25269=CARTESIAN_POINT('Ctrl Pts',(-0.99133911172057,1.48977648468554,7.21244696501856));
#25270=CARTESIAN_POINT('Ctrl Pts',(-1.03697892191269,1.44790768513415,7.22152145851107));
#25271=CARTESIAN_POINT('Ctrl Pts',(-1.0804266997828,1.40346470822021,7.2306710363693));
#25272=CARTESIAN_POINT('Ctrl Pts',(-1.12150612234599,1.35666626833897,7.23991063613496));
#25273=CARTESIAN_POINT('Ctrl Pts',(-1.12930267296081,1.34778429331443,7.24166423934404));
#25274=CARTESIAN_POINT('Ctrl Pts',(-1.13701438607344,1.338816634524,7.24342123717376));
#25275=CARTESIAN_POINT('Ctrl Pts',(-1.14462934985433,1.32977774514085,7.24517924126443));
#25276=CARTESIAN_POINT('Ctrl Pts',(-1.18689780114357,1.27960549657953,7.25493741115345));
#25277=CARTESIAN_POINT('Ctrl Pts',(-1.22626964349749,1.22715044372182,7.26474446593405));
#25278=CARTESIAN_POINT('Ctrl Pts',(-1.2626041554744,1.17270468062558,7.27462138727731));
#25279=CARTESIAN_POINT('Ctrl Pts',(-1.29870272792618,1.11861246314731,7.28443417245898));
#25280=CARTESIAN_POINT('Ctrl Pts',(-1.33180351900955,1.06255418531111,7.29431591978697));
#25281=CARTESIAN_POINT('Ctrl Pts',(-1.36171904589852,1.00480435475497,7.30428720484495));
#25282=CARTESIAN_POINT('Ctrl Pts',(-1.39100085763464,0.948277866941019,
7.31404726332289));
#25283=CARTESIAN_POINT('Ctrl Pts',(-1.41723097430462,0.890129769006774,
7.32389310626744));
#25284=CARTESIAN_POINT('Ctrl Pts',(-1.44018415693848,0.83062133555421,7.33384402917814));
#25285=CARTESIAN_POINT('Ctrl Pts',(-1.44632047771148,0.814712307068312,
7.33650431624776));
#25286=CARTESIAN_POINT('Ctrl Pts',(-1.45222231211246,0.798706119319694,
7.33917211349499));
#25287=CARTESIAN_POINT('Ctrl Pts',(-1.45788473508532,0.78260794455952,7.34184778960142));
#25288=CARTESIAN_POINT('Ctrl Pts',(-1.46140114941093,0.772610836852428,
7.34350940792919));
#25289=CARTESIAN_POINT('Ctrl Pts',(-1.4648248277114,0.762579164108622,7.34517391187186));
#25290=CARTESIAN_POINT('Ctrl Pts',(-1.46815093425694,0.752525994362274,
7.34683944075502));
#25291=CARTESIAN_POINT('Ctrl Pts',(-1.4875809575628,0.693798674658319,7.35656891411169));
#25292=CARTESIAN_POINT('Ctrl Pts',(-1.50372373374688,0.634230525264841,
7.36635120065226));
#25293=CARTESIAN_POINT('Ctrl Pts',(-1.51642546703182,0.574066612526935,
7.37620769393241));
#25294=CARTESIAN_POINT('Ctrl Pts',(-1.52890893161854,0.514936566476241,
7.385894811592));
#25295=CARTESIAN_POINT('Ctrl Pts',(-1.53806859003218,0.455230176794947,
7.39565360754218));
#25296=CARTESIAN_POINT('Ctrl Pts',(-1.54370934814325,0.395188284726392,
7.40550439129109));
#25297=CARTESIAN_POINT('Ctrl Pts',(-1.54918565956382,0.33689681170573,7.41506799222619));
#25298=CARTESIAN_POINT('Ctrl Pts',(-1.55134510253712,0.278288450517533,
7.42471829564676));
#25299=CARTESIAN_POINT('Ctrl Pts',(-1.54996382900015,0.219602494440036,
7.43447388607445));
#25300=CARTESIAN_POINT('Ctrl Pts',(-1.54949240817649,0.199573310494113,
7.43780341375428));
#25301=CARTESIAN_POINT('Ctrl Pts',(-1.5486081708139,0.179535297751125,7.44114520545616));
#25302=CARTESIAN_POINT('Ctrl Pts',(-1.54730100999696,0.159498697368912,
7.4445));
#25303=CARTESIAN_POINT('',(-1.49051052577446,1.26051379553366,7.046));
#25304=CARTESIAN_POINT('Origin',(0.,0.,7.046));
#25305=CARTESIAN_POINT('Ctrl Pts',(-1.90742224034152,0.000616434489977578,
7.09553262952215));
#25306=CARTESIAN_POINT('Ctrl Pts',(-1.90876164805009,0.0329240599094907,
7.09432940051696));
#25307=CARTESIAN_POINT('Ctrl Pts',(-1.90921779267002,0.0652320529994964,
7.09312819770054));
#25308=CARTESIAN_POINT('Ctrl Pts',(-1.90877477964874,0.0975109530601205,
7.09192862283081));
#25309=CARTESIAN_POINT('Ctrl Pts',(-1.90781024899833,0.16778877103618,7.08931690111213));
#25310=CARTESIAN_POINT('Ctrl Pts',(-1.90258719753853,0.237928585345474,
7.08671289622934));
#25311=CARTESIAN_POINT('Ctrl Pts',(-1.89333689480301,0.307653748465392,
7.08411249814515));
#25312=CARTESIAN_POINT('Ctrl Pts',(-1.88389965579861,0.378787964046921,
7.0814595494873));
#25313=CARTESIAN_POINT('Ctrl Pts',(-1.87027048866354,0.449491484193812,
7.0788103548782));
#25314=CARTESIAN_POINT('Ctrl Pts',(-1.8526408196263,0.519466411196971,7.0761605500361));
#25315=CARTESIAN_POINT('Ctrl Pts',(-1.84839799409914,0.536306852496432,
7.07552283757523));
#25316=CARTESIAN_POINT('Ctrl Pts',(-1.8439232315986,0.553105040705889,7.07488508977019));
#25317=CARTESIAN_POINT('Ctrl Pts',(-1.83921877202327,0.569856697426902,
7.07424724578707));
#25318=CARTESIAN_POINT('Ctrl Pts',(-1.83514299244073,0.584369748149054,
7.07369464002192));
#25319=CARTESIAN_POINT('Ctrl Pts',(-1.83089368872409,0.598851100707912,
7.07314183740804));
#25320=CARTESIAN_POINT('Ctrl Pts',(-1.82648012174354,0.613273349358239,
7.07258974257699));
#25321=CARTESIAN_POINT('Ctrl Pts',(-1.80525925753629,0.682616939592868,
7.06993521631944));
#25322=CARTESIAN_POINT('Ctrl Pts',(-1.78021580797096,0.750706522102631,
7.06729279368472));
#25323=CARTESIAN_POINT('Ctrl Pts',(-1.75159954554489,0.817253861437449,
7.06465826007958));
#25324=CARTESIAN_POINT('Ctrl Pts',(-1.72257788914062,0.884743947600279,
7.06198640419794));
#25325=CARTESIAN_POINT('Ctrl Pts',(-1.68988110151814,0.950648721336099,
7.05932266244995));
#25326=CARTESIAN_POINT('Ctrl Pts',(-1.65371662519363,1.01465825897231,7.05666263857406));
#25327=CARTESIAN_POINT('Ctrl Pts',(-1.61767133058481,1.07845685019671,7.05401138093072));
#25328=CARTESIAN_POINT('Ctrl Pts',(-1.57818065931587,1.14037360389397,7.051363816695));
#25329=CARTESIAN_POINT('Ctrl Pts',(-1.53540446982221,1.20007853919048,7.04871559292653));
#25330=CARTESIAN_POINT('Ctrl Pts',(-1.52078518671176,1.2204834271088,7.04781053023934));
#25331=CARTESIAN_POINT('Ctrl Pts',(-1.50578179227618,1.24062970905854,7.04690539051781));
#25332=CARTESIAN_POINT('Ctrl Pts',(-1.49039960333531,1.26050328917698,7.046));
#25333=CARTESIAN_POINT('',(-1.,-1.22464679914735E-16,8.));
#25334=CARTESIAN_POINT('',(-1.5,-1.83697019872103E-16,7.5));
#25335=CARTESIAN_POINT('Origin',(0.,0.,8.));
#25336=CARTESIAN_POINT('Ctrl Pts',(1.13509973994373,-1.59049193030951,-0.230074082272067));
#25337=CARTESIAN_POINT('Ctrl Pts',(1.66385265555159,-1.21313239420412,-0.193036768839232));
#25338=CARTESIAN_POINT('Ctrl Pts',(2.30633309595034,0.10379526882931,-0.11896214197356));
#25339=CARTESIAN_POINT('Ctrl Pts',(1.1618831159781,1.99754257541113,-0.00785020167505245));
#25340=CARTESIAN_POINT('Ctrl Pts',(-1.04657265959996,2.05782619857144,0.103261738623455));
#25341=CARTESIAN_POINT('Ctrl Pts',(-2.29698513032901,0.238308494988224,
0.214373678921962));
#25342=CARTESIAN_POINT('Ctrl Pts',(-1.44610949780919,-1.80077244555215,
0.32548561922047));
#25343=CARTESIAN_POINT('Ctrl Pts',(0.727982080133343,-2.19148935509534,
0.436597559518978));
#25344=CARTESIAN_POINT('Ctrl Pts',(2.23595404085407,-0.577589325353924,
0.547709499817485));
#25345=CARTESIAN_POINT('Ctrl Pts',(1.69824597043106,1.56497940407905,0.658821440115993));
#25346=CARTESIAN_POINT('Ctrl Pts',(-0.393241729595879,2.27560136836119,
0.7699333804145));
#25347=CARTESIAN_POINT('Ctrl Pts',(-2.12493397204,0.90429099396703,0.881045320713008));
#25348=CARTESIAN_POINT('Ctrl Pts',(-1.91248731439823,-1.29440519809075,
0.992157261011514));
#25349=CARTESIAN_POINT('Ctrl Pts',(0.0497351526023427,-2.30880745912378,
1.10326920131002));
#25350=CARTESIAN_POINT('Ctrl Pts',(1.96645238083605,-1.21084445058012,1.21438114160853));
#25351=CARTESIAN_POINT('Ctrl Pts',(2.0840238587571,0.994948952062592,1.32549308190704));
#25352=CARTESIAN_POINT('Ctrl Pts',(0.294879848465431,2.29044125875909,1.43660502220554));
#25353=CARTESIAN_POINT('Ctrl Pts',(-1.76405540105404,1.49036437523231,1.54771696250405));
#25354=CARTESIAN_POINT('Ctrl Pts',(-2.20902124244616,-0.673277315499274,
1.65882890280256));
#25355=CARTESIAN_POINT('Ctrl Pts',(-0.63290935858251,-2.22092378987733,
1.76994084310107));
#25356=CARTESIAN_POINT('Ctrl Pts',(1.5222639082646,-1.73660290660664,1.88105278339957));
#25357=CARTESIAN_POINT('Ctrl Pts',(2.28468753295219,0.336570763856544,1.99216472369808));
#25358=CARTESIAN_POINT('Ctrl Pts',(0.956804884638204,2.10180906822536,2.10327666399659));
#25359=CARTESIAN_POINT('Ctrl Pts',(-1.24647766157407,1.94406029583798,2.2143886042951));
#25360=CARTESIAN_POINT('Ctrl Pts',(-2.30933289737607,0.00765190922063762,
2.3255005445936));
#25361=CARTESIAN_POINT('Ctrl Pts',(-1.25933333160116,-1.9357573546638,2.43661248489211));
#25362=CARTESIAN_POINT('Ctrl Pts',(0.942855455692524,-2.10810354889204,
2.54772442519062));
#25363=CARTESIAN_POINT('Ctrl Pts',(2.28240695194457,-0.35170369161106,2.65883636548913));
#25364=CARTESIAN_POINT('Ctrl Pts',(1.53373873309094,1.72647689788489,2.76994830578763));
#25365=CARTESIAN_POINT('Ctrl Pts',(-0.618177691355928,2.22506928503553,
2.88106024608615));
#25366=CARTESIAN_POINT('Ctrl Pts',(-2.20451099698397,0.687901333838673,
2.99217218638465));
#25367=CARTESIAN_POINT('Ctrl Pts',(-1.77389315295183,-1.47864128941955,
3.10328412668316));
#25368=CARTESIAN_POINT('Ctrl Pts',(0.279694972942425,-2.29234545893725,
3.21439606698166));
#25369=CARTESIAN_POINT('Ctrl Pts',(2.07738458076118,-1.00873697491097,3.32550800728017));
#25370=CARTESIAN_POINT('Ctrl Pts',(1.97443353669272,1.1977851185115,3.43661994757868));
#25371=CARTESIAN_POINT('Ctrl Pts',(0.0650338075591902,2.30842967941821,
3.54773188787719));
#25372=CARTESIAN_POINT('Ctrl Pts',(-1.90386665125239,1.30704581219857,3.65884382817569));
#25373=CARTESIAN_POINT('Ctrl Pts',(-2.13088147818969,-0.890180378860142,
3.7699557684742));
#25374=CARTESIAN_POINT('Ctrl Pts',(-0.408310273068383,-2.2729627585538,
3.88106770877271));
#25375=CARTESIAN_POINT('Ctrl Pts',(1.6878321574451,-1.57616610457607,3.99217964907122));
#25376=CARTESIAN_POINT('Ctrl Pts',(2.23974323019256,0.562696404915903,4.10329158936972));
#25377=CARTESIAN_POINT('Ctrl Pts',(0.742468479097436,2.18673673263618,4.21440352966824));
#25378=CARTESIAN_POINT('Ctrl Pts',(-1.43410551503643,1.81008794060395,4.32551546996673));
#25379=CARTESIAN_POINT('Ctrl Pts',(-2.29858772583325,-0.222646468261011,
4.43662741026525));
#25380=CARTESIAN_POINT('Ctrl Pts',(-1.06004610686433,-2.05167717429874,
4.54773935056375));
#25381=CARTESIAN_POINT('Ctrl Pts',(1.14835286831205,-2.00358745066383,4.65885129086226));
#25382=CARTESIAN_POINT('Ctrl Pts',(2.30610086989477,-0.122375538925838,
4.76996323116077));
#25383=CARTESIAN_POINT('Ctrl Pts',(1.35395110677505,1.87080018895779,4.88107517145928));
#25384=CARTESIAN_POINT('Ctrl Pts',(-0.836955550366062,2.15234346911026,
4.99218711175778));
#25385=CARTESIAN_POINT('Ctrl Pts',(-2.26211489466594,0.464664680140549,
5.10329905205629));
#25386=CARTESIAN_POINT('Ctrl Pts',(-1.61762005706343,-1.64814504446985,
5.2144109923548));
#25387=CARTESIAN_POINT('Ctrl Pts',(0.506867541264277,-2.25303406293758,
5.3255229326533));
#25388=CARTESIAN_POINT('Ctrl Pts',(2.16761217480869,-0.796576982199858,
5.43663487295182));
#25389=CARTESIAN_POINT('Ctrl Pts',(1.84516460593919,1.38868385957575,5.54774681325032));
#25390=CARTESIAN_POINT('Ctrl Pts',(-0.165459925935554,2.30341092165264,
5.65885875354883));
#25391=CARTESIAN_POINT('Ctrl Pts',(-2.02470376163623,1.11069974665188,5.76997069384733));
#25392=CARTESIAN_POINT('Ctrl Pts',(-2.03150206860296,-1.09820982237999,
5.88108263414585));
#25393=CARTESIAN_POINT('Ctrl Pts',(-0.179645428808579,-2.30235098638037,
5.99219457444435));
#25394=CARTESIAN_POINT('Ctrl Pts',(1.83658550522895,-1.40001438181273,6.10330651474285));
#25395=CARTESIAN_POINT('Ctrl Pts',(2.17246271157681,0.783202663677277,6.21441845504137));
#25396=CARTESIAN_POINT('Ctrl Pts',(0.520757933621259,2.24989134978725,6.32553039533987));
#25397=CARTESIAN_POINT('Ctrl Pts',(-1.60748926038381,1.65803443249082,6.43664233563838));
#25398=CARTESIAN_POINT('Ctrl Pts',(-2.26483986170582,-0.450648314453544,
6.54775427593688));
#25399=CARTESIAN_POINT('Ctrl Pts',(-0.850371985170964,-2.14729633892256,
6.6588662162354));
#25400=CARTESIAN_POINT('Ctrl Pts',(1.34274482878903,-1.87882089420371,6.7699781565339));
#25401=CARTESIAN_POINT('Ctrl Pts',(2.30616083080651,0.107634649639171,6.88109009683241));
#25402=CARTESIAN_POINT('Ctrl Pts',(1.16193045799902,1.99751503787814,6.99220203713092));
#25403=CARTESIAN_POINT('Ctrl Pts',(-1.04999517826429,2.05607780322851,7.10331397742942));
#25404=CARTESIAN_POINT('Ctrl Pts',(-1.87709151778098,0.84653605896511,7.1773886042951));
#25405=CARTESIAN_POINT('Ctrl Pts',(-1.94370052943366,0.200360305148756,
7.21442591772793));
#25406=CARTESIAN_POINT('Ctrl Pts',(1.05793541951256,-1.48236995244729,-0.153382721514712));
#25407=CARTESIAN_POINT('Ctrl Pts',(1.55074360006928,-1.13066339742992,-0.116345408081876));
#25408=CARTESIAN_POINT('Ctrl Pts',(2.14954808422461,0.0967392444982914,
-0.0422707812162042));
#25409=CARTESIAN_POINT('Ctrl Pts',(1.08289805597856,1.8617492085907,0.0688411590823027));
#25410=CARTESIAN_POINT('Ctrl Pts',(-0.975426428816855,1.91793473829667,
0.179953099380811));
#25411=CARTESIAN_POINT('Ctrl Pts',(-2.14083559528361,0.222108233089066,
0.291065039679317));
#25412=CARTESIAN_POINT('Ctrl Pts',(-1.34780266824982,-1.6783555537827,0.402176979977826));
#25413=CARTESIAN_POINT('Ctrl Pts',(0.678493704334455,-2.04251144516605,
0.513288920276332));
#25414=CARTESIAN_POINT('Ctrl Pts',(2.08395341218121,-0.538324680837788,
0.624400860574841));
#25415=CARTESIAN_POINT('Ctrl Pts',(1.58279885012795,1.4585917731467,0.735512800873347));
#25416=CARTESIAN_POINT('Ctrl Pts',(-0.366509073634787,2.12090550597771,
0.846624741171857));
#25417=CARTESIAN_POINT('Ctrl Pts',(-1.9804805111294,0.842817100910752,0.957736681470361));
#25418=CARTESIAN_POINT('Ctrl Pts',(-1.78247602221336,-1.20641125891655,
1.06884862176887));
#25419=CARTESIAN_POINT('Ctrl Pts',(0.0463541464078725,-2.15185423966612,
1.17996056206738));
#25420=CARTESIAN_POINT('Ctrl Pts',(1.83277253201941,-1.12853098869745,1.29107250236589));
#25421=CARTESIAN_POINT('Ctrl Pts',(1.94235147600127,0.927312111837943,1.40218444266439));
#25422=CARTESIAN_POINT('Ctrl Pts',(0.274833853990247,2.13473657748725,1.5132963829629));
#25423=CARTESIAN_POINT('Ctrl Pts',(-1.6441345417364,1.38904908974441,1.62440832326141));
#25424=CARTESIAN_POINT('Ctrl Pts',(-2.05885151110621,-0.627507781172011,
1.73552026355991));
#25425=CARTESIAN_POINT('Ctrl Pts',(-0.589884046505544,-2.06994492084524,
1.84663220385842));
#25426=CARTESIAN_POINT('Ctrl Pts',(1.4187800857734,-1.6185482736686,1.95774414415693));
#25427=CARTESIAN_POINT('Ctrl Pts',(2.12937399117781,0.313690612134129,2.06885608445544));
#25428=CARTESIAN_POINT('Ctrl Pts',(0.891761086185737,1.95892764316774,2.17996802475395));
#25429=CARTESIAN_POINT('Ctrl Pts',(-1.16174184647048,1.81190266569614,2.29107996505245));
#25430=CARTESIAN_POINT('Ctrl Pts',(-2.15234395851487,0.00713173081318942,
2.40219190535096));
#25431=CARTESIAN_POINT('Ctrl Pts',(-1.17372358532974,-1.80416416021932,
2.51330384564946));
#25432=CARTESIAN_POINT('Ctrl Pts',(0.878759942370547,-1.96479422370721,
2.62441578594798));
#25433=CARTESIAN_POINT('Ctrl Pts',(2.1272484445495,-0.327794800258781,2.73552772624649));
#25434=CARTESIAN_POINT('Ctrl Pts',(1.42947484958074,1.60911063316174,2.84663966654499));
#25435=CARTESIAN_POINT('Ctrl Pts',(-0.576153841133258,2.07380860436568,
2.9577516068435));
#25436=CARTESIAN_POINT('Ctrl Pts',(-2.0546478730846,0.641137655651238,3.068863547142));
#25437=CARTESIAN_POINT('Ctrl Pts',(-1.65330352117917,-1.37812294178502,
3.17997548744051));
#25438=CARTESIAN_POINT('Ctrl Pts',(0.260681249517398,-2.1365113297345,3.29108742773902));
#25439=CARTESIAN_POINT('Ctrl Pts',(1.93616353752793,-0.940162821976462,
3.40219936803753));
#25440=CARTESIAN_POINT('Ctrl Pts',(1.84021112721267,1.11635943278533,3.51331130833604));
#25441=CARTESIAN_POINT('Ctrl Pts',(0.0606127955645832,2.15150214150485,
3.62442324863454));
#25442=CARTESIAN_POINT('Ctrl Pts',(-1.77444139357172,1.21819256140342,3.73553518893305));
#25443=CARTESIAN_POINT('Ctrl Pts',(-1.98602370455295,-0.829665728403687,
3.84664712923155));
#25444=CARTESIAN_POINT('Ctrl Pts',(-0.380553254334539,-2.11844626942319,
3.95775906953007));
#25445=CARTESIAN_POINT('Ctrl Pts',(1.57309297035165,-1.46901799937757,4.06887100982856));
#25446=CARTESIAN_POINT('Ctrl Pts',(2.08748501162692,0.524444184281487,4.17998295012709));
#25447=CARTESIAN_POINT('Ctrl Pts',(0.691995314832617,2.038081906987,4.29109489042558));
#25448=CARTESIAN_POINT('Ctrl Pts',(-1.33661471876519,1.68703777951035,4.4022068307241));
#25449=CARTESIAN_POINT('Ctrl Pts',(-2.14232924600648,-0.207510914251802,
4.5133187710226));
#25450=CARTESIAN_POINT('Ctrl Pts',(-0.987983948286119,-1.91220372599474,
4.62443071132112));
#25451=CARTESIAN_POINT('Ctrl Pts',(1.07028759741094,-1.86738315194504,4.73554265161961));
#25452=CARTESIAN_POINT('Ctrl Pts',(2.14933164494543,-0.114056423903322,
4.84665459191812));
#25453=CARTESIAN_POINT('Ctrl Pts',(1.26190922413262,1.74362279637852,4.95776653221663));
#25454=CARTESIAN_POINT('Ctrl Pts',(-0.780059135009386,2.00602670479084,
5.06887847251514));
#25455=CARTESIAN_POINT('Ctrl Pts',(-2.10833584561709,0.433076676893185,
5.17999041281365));
#25456=CARTESIAN_POINT('Ctrl Pts',(-1.50765390340601,-1.53610379571154,
5.29110235311216));
#25457=CARTESIAN_POINT('Ctrl Pts',(0.472410578590484,-2.0998723307505,5.40221429341067));
#25458=CARTESIAN_POINT('Ctrl Pts',(2.02025744064608,-0.742425510448462,
5.51332623370916));
#25459=CARTESIAN_POINT('Ctrl Pts',(1.71972992571626,1.29428083705086,5.62443817400769));
#25460=CARTESIAN_POINT('Ctrl Pts',(-0.154211925170411,2.14682455995381,
5.73555011430617));
#25461=CARTESIAN_POINT('Ctrl Pts',(-1.88706397163077,1.03519414292605,5.8466620546047));
#25462=CARTESIAN_POINT('Ctrl Pts',(-1.89340012825184,-1.02355328634819,
5.95777399490319));
#25463=CARTESIAN_POINT('Ctrl Pts',(-0.167433094557426,-2.14583667930556,
6.0688859352017));
#25464=CARTESIAN_POINT('Ctrl Pts',(1.71173403408707,-1.3048411079894,6.17999787550022));
#25465=CARTESIAN_POINT('Ctrl Pts',(2.02477823689865,0.729960380928156,6.29110981579872));
#25466=CARTESIAN_POINT('Ctrl Pts',(0.485356699136765,2.09694325990492,6.40222175609723));
#25467=CARTESIAN_POINT('Ctrl Pts',(-1.49821180042767,1.54532090104292,6.51333369639574));
#25468=CARTESIAN_POINT('Ctrl Pts',(-2.11087556882117,-0.420013146710507,
6.62444563669424));
#25469=CARTESIAN_POINT('Ctrl Pts',(-0.792563517738235,-2.00132267958093,
6.73555757699275));
#25470=CARTESIAN_POINT('Ctrl Pts',(1.2514647512946,-1.75109825238519,6.84666951729126));
#25471=CARTESIAN_POINT('Ctrl Pts',(2.1493875297017,0.100317623388547,6.95778145758976));
#25472=CARTESIAN_POINT('Ctrl Pts',(1.08294217967889,1.86172354306503,7.06889339788828));
#25473=CARTESIAN_POINT('Ctrl Pts',(-0.978616283938414,1.91630519923899,
7.18000533818678));
#25474=CARTESIAN_POINT('Ctrl Pts',(-1.74948643933749,0.788988358607273,
7.25407996505245));
#25475=CARTESIAN_POINT('Ctrl Pts',(-1.8115673562881,0.186739769222141,7.29111727848529));
#25476=CARTESIAN_POINT('Ctrl Pts',(0.980771099081382,-1.37424797458506,
-0.0766913607573567));
#25477=CARTESIAN_POINT('Ctrl Pts',(1.43763454458697,-1.04819440065571,-0.0396540473245209));
#25478=CARTESIAN_POINT('Ctrl Pts',(1.99276307249889,0.0896832201672716,
0.034420579541151));
#25479=CARTESIAN_POINT('Ctrl Pts',(1.00391299597902,1.72595584177028,0.145532519839658));
#25480=CARTESIAN_POINT('Ctrl Pts',(-0.904280198033752,1.77804327802189,
0.256644460138166));
#25481=CARTESIAN_POINT('Ctrl Pts',(-1.98468606023822,0.205907971189911,
0.367756400436673));
#25482=CARTESIAN_POINT('Ctrl Pts',(-1.24949583869046,-1.55593866201325,
0.478868340735181));
#25483=CARTESIAN_POINT('Ctrl Pts',(0.629005328535562,-1.89353353523676,
0.589980281033688));
#25484=CARTESIAN_POINT('Ctrl Pts',(1.93195278350834,-0.499060036321655,
0.701092221332196));
#25485=CARTESIAN_POINT('Ctrl Pts',(1.46735172982485,1.35220414221434,0.812204161630702));
#25486=CARTESIAN_POINT('Ctrl Pts',(-0.339776417673698,1.96620964359423,
0.923316101929211));
#25487=CARTESIAN_POINT('Ctrl Pts',(-1.8360270502188,0.781343207854476,1.03442804222772));
#25488=CARTESIAN_POINT('Ctrl Pts',(-1.65246473002849,-1.11841731974236,
1.14553998252623));
#25489=CARTESIAN_POINT('Ctrl Pts',(0.0429731402134002,-1.99490102020845,
1.25665192282473));
#25490=CARTESIAN_POINT('Ctrl Pts',(1.69909268320277,-1.04621752681478,1.36776386312324));
#25491=CARTESIAN_POINT('Ctrl Pts',(1.80067909324543,0.859675271613291,1.47887580342175));
#25492=CARTESIAN_POINT('Ctrl Pts',(0.254787859515066,1.97903189621542,1.58998774372026));
#25493=CARTESIAN_POINT('Ctrl Pts',(-1.52421368241876,1.2877338042565,1.70109968401876));
#25494=CARTESIAN_POINT('Ctrl Pts',(-1.90868177976625,-0.581738246844747,
1.81221162431727));
#25495=CARTESIAN_POINT('Ctrl Pts',(-0.54685873442858,-1.91896605181315,
1.92332356461578));
#25496=CARTESIAN_POINT('Ctrl Pts',(1.3152962632822,-1.50049364073057,2.03443550491428));
#25497=CARTESIAN_POINT('Ctrl Pts',(1.97406044940342,0.290810460411716,2.14554744521279));
#25498=CARTESIAN_POINT('Ctrl Pts',(0.826717287733271,1.81604621811011,2.2566593855113));
#25499=CARTESIAN_POINT('Ctrl Pts',(-1.0770060313669,1.6797450355543,2.36777132580981));
#25500=CARTESIAN_POINT('Ctrl Pts',(-1.99535501965367,0.00661155240574004,
2.47888326610832));
#25501=CARTESIAN_POINT('Ctrl Pts',(-1.08811383905831,-1.67257096577485,
2.58999520640682));
#25502=CARTESIAN_POINT('Ctrl Pts',(0.814664429048569,-1.82148489852237,
2.70110714670533));
#25503=CARTESIAN_POINT('Ctrl Pts',(1.97208993715443,-0.303885908906504,
2.81221908700384));
#25504=CARTESIAN_POINT('Ctrl Pts',(1.32521096607054,1.49174436843859,2.92333102730234));
#25505=CARTESIAN_POINT('Ctrl Pts',(-0.534129990910586,1.92254792369583,
3.03444296760085));
#25506=CARTESIAN_POINT('Ctrl Pts',(-1.90478474918523,0.594373977463801,
3.14555490789936));
#25507=CARTESIAN_POINT('Ctrl Pts',(-1.53271388940651,-1.27760459415048,
3.25666684819786));
#25508=CARTESIAN_POINT('Ctrl Pts',(0.241667526092368,-1.98067720053176,
3.36777878849638));
#25509=CARTESIAN_POINT('Ctrl Pts',(1.79494249429468,-0.871588669041957,
3.47889072879488));
#25510=CARTESIAN_POINT('Ctrl Pts',(1.70598871773261,1.03493374705916,3.59000266909339));
#25511=CARTESIAN_POINT('Ctrl Pts',(0.0561917835699789,1.99457460359148,
3.70111460939189));
#25512=CARTESIAN_POINT('Ctrl Pts',(-1.64501613589106,1.12933931060827,3.81222654969041));
#25513=CARTESIAN_POINT('Ctrl Pts',(-1.8411659309162,-0.769151077947235,
3.92333848998891));
#25514=CARTESIAN_POINT('Ctrl Pts',(-0.352796235600697,-1.96392978029257,
4.03445043028742));
#25515=CARTESIAN_POINT('Ctrl Pts',(1.45835378325819,-1.36186989417907,4.14556237058593));
#25516=CARTESIAN_POINT('Ctrl Pts',(1.93522679306129,0.486191963647073,4.25667431088443));
#25517=CARTESIAN_POINT('Ctrl Pts',(0.641522150567798,1.88942708133782,4.36778625118295));
#25518=CARTESIAN_POINT('Ctrl Pts',(-1.23912392249396,1.56398761841675,4.47889819148144));
#25519=CARTESIAN_POINT('Ctrl Pts',(-1.9860707661797,-0.192375360242598,
4.59001013177996));
#25520=CARTESIAN_POINT('Ctrl Pts',(-0.915921789707908,-1.77273027769074,
4.70112207207846));
#25521=CARTESIAN_POINT('Ctrl Pts',(0.992222326509824,-1.73117885322625,
4.81223401237697));
#25522=CARTESIAN_POINT('Ctrl Pts',(1.99256241999608,-0.105737308880805,
4.92334595267548));
#25523=CARTESIAN_POINT('Ctrl Pts',(1.1698673414902,1.61644540379926,5.03445789297399));
#25524=CARTESIAN_POINT('Ctrl Pts',(-0.723162719652709,1.85970994047142,
5.1455698332725));
#25525=CARTESIAN_POINT('Ctrl Pts',(-1.95455679656824,0.401488673645819,
5.25668177357099));
#25526=CARTESIAN_POINT('Ctrl Pts',(-1.39768774974859,-1.42406254695323,
5.36779371386952));
#25527=CARTESIAN_POINT('Ctrl Pts',(0.437953615916691,-1.94671059856343,
5.47890565416801));
#25528=CARTESIAN_POINT('Ctrl Pts',(1.87290270648346,-0.688274038697066,
5.59001759446653));
#25529=CARTESIAN_POINT('Ctrl Pts',(1.59429524549334,1.19987781452597,5.70112953476503));
#25530=CARTESIAN_POINT('Ctrl Pts',(-0.142963924405265,1.99023819825497,
5.81224147506354));
#25531=CARTESIAN_POINT('Ctrl Pts',(-1.74942418162531,0.959688539200224,
5.92335341536204));
#25532=CARTESIAN_POINT('Ctrl Pts',(-1.75529818790071,-0.948896750316397,
6.03446535566056));
#25533=CARTESIAN_POINT('Ctrl Pts',(-0.155220760306272,-1.98932237223074,
6.14557729595905));
#25534=CARTESIAN_POINT('Ctrl Pts',(1.58688256294519,-1.20966783416606,6.25668923625758));
#25535=CARTESIAN_POINT('Ctrl Pts',(1.8770937622205,0.676718098179033,6.36780117655607));
#25536=CARTESIAN_POINT('Ctrl Pts',(0.449955464652266,1.94399517002259,6.47891311685458));
#25537=CARTESIAN_POINT('Ctrl Pts',(-1.38893434047152,1.43260736959501,6.59002505715309));
#25538=CARTESIAN_POINT('Ctrl Pts',(-1.95691127593653,-0.389377978967469,
6.7011369974516));
#25539=CARTESIAN_POINT('Ctrl Pts',(-0.734755050305503,-1.8553490202393,
6.8122489377501));
#25540=CARTESIAN_POINT('Ctrl Pts',(1.16018467380016,-1.62337561056666,6.92336087804862));
#25541=CARTESIAN_POINT('Ctrl Pts',(1.99261422859689,0.0930005971379224,
7.03447281834711));
#25542=CARTESIAN_POINT('Ctrl Pts',(1.00395390135875,1.72593204825193,7.14558475864564));
#25543=CARTESIAN_POINT('Ctrl Pts',(-0.907237389612538,1.77653259524947,
7.25669669894413));
#25544=CARTESIAN_POINT('Ctrl Pts',(-1.62188136089401,0.731440658249439,
7.33077132580981));
#25545=CARTESIAN_POINT('Ctrl Pts',(-1.67943418314253,0.173119233295526,
7.36780863924264));
#25546=CARTESIAN_POINT('Ctrl Pts',(0.903606778650207,-1.26612599672284,
-1.38777878078145E-15));
#25547=CARTESIAN_POINT('Ctrl Pts',(1.32452548910467,-0.965725403881512,
0.0370373134328344));
#25548=CARTESIAN_POINT('Ctrl Pts',(1.83597806077316,0.082627195836251,0.111111940298506));
#25549=CARTESIAN_POINT('Ctrl Pts',(0.924927935979477,1.59016247494986,0.222223880597014));
#25550=CARTESIAN_POINT('Ctrl Pts',(-0.833133967250649,1.63815181774712,
0.333335820895521));
#25551=CARTESIAN_POINT('Ctrl Pts',(-1.82853652519283,0.189707709290757,
0.444447761194028));
#25552=CARTESIAN_POINT('Ctrl Pts',(-1.15118900913109,-1.43352177024381,
0.555559701492536));
#25553=CARTESIAN_POINT('Ctrl Pts',(0.579516952736672,-1.74455562530747,
0.666671641791043));
#25554=CARTESIAN_POINT('Ctrl Pts',(1.77995215483547,-0.45979539180552,0.777783582089551));
#25555=CARTESIAN_POINT('Ctrl Pts',(1.35190460952174,1.24581651128198,0.888895522388059));
#25556=CARTESIAN_POINT('Ctrl Pts',(-0.313043761712607,1.81151378121076,
1.00000746268657));
#25557=CARTESIAN_POINT('Ctrl Pts',(-1.6915735893082,0.719869314798195,1.11111940298507));
#25558=CARTESIAN_POINT('Ctrl Pts',(-1.52245343784362,-1.03042338056816,
1.22223134328358));
#25559=CARTESIAN_POINT('Ctrl Pts',(0.0395921340189295,-1.83794780075079,
1.33334328358209));
#25560=CARTESIAN_POINT('Ctrl Pts',(1.56541283438613,-0.96390406493211,1.44445522388059));
#25561=CARTESIAN_POINT('Ctrl Pts',(1.65900671048959,0.792038431388639,1.55556716417911));
#25562=CARTESIAN_POINT('Ctrl Pts',(0.234741865039883,1.82332721494359,1.66667910447761));
#25563=CARTESIAN_POINT('Ctrl Pts',(-1.40429282310112,1.18641851876859,1.77779104477612));
#25564=CARTESIAN_POINT('Ctrl Pts',(-1.7585120484263,-0.535968712517482,
1.88890298507462));
#25565=CARTESIAN_POINT('Ctrl Pts',(-0.503833422351614,-1.76798718278107,
2.00001492537314));
#25566=CARTESIAN_POINT('Ctrl Pts',(1.211812440791,-1.38243900779253,2.11112686567164));
#25567=CARTESIAN_POINT('Ctrl Pts',(1.81874690762903,0.2679303086893,2.22223880597015));
#25568=CARTESIAN_POINT('Ctrl Pts',(0.761673489280804,1.67316479305249,2.33335074626865));
#25569=CARTESIAN_POINT('Ctrl Pts',(-0.99227021626331,1.54758740541246,2.44446268656716));
#25570=CARTESIAN_POINT('Ctrl Pts',(-1.83836608079246,0.00609137399829168,
2.55557462686567));
#25571=CARTESIAN_POINT('Ctrl Pts',(-1.00250409278689,-1.54097777133038,
2.66668656716418));
#25572=CARTESIAN_POINT('Ctrl Pts',(0.750568915726592,-1.67817557333754,
2.77779850746269));
#25573=CARTESIAN_POINT('Ctrl Pts',(1.81693142975936,-0.279977017554228,
2.8889104477612));
#25574=CARTESIAN_POINT('Ctrl Pts',(1.22094708256035,1.37437810371544,3.0000223880597));
#25575=CARTESIAN_POINT('Ctrl Pts',(-0.492106140687917,1.77128724302598,
3.11113432835821));
#25576=CARTESIAN_POINT('Ctrl Pts',(-1.75492162528586,0.547610299276366,
3.22224626865671));
#25577=CARTESIAN_POINT('Ctrl Pts',(-1.41212425763385,-1.17708624651594,
3.33335820895523));
#25578=CARTESIAN_POINT('Ctrl Pts',(0.222653802667342,-1.82484307132901,
3.44447014925373));
#25579=CARTESIAN_POINT('Ctrl Pts',(1.65372145106143,-0.803014516107455,
3.55558208955224));
#25580=CARTESIAN_POINT('Ctrl Pts',(1.57176630825256,0.953508061332994,3.66669402985075));
#25581=CARTESIAN_POINT('Ctrl Pts',(0.0517707715753711,1.83764706567811,
3.77780597014925));
#25582=CARTESIAN_POINT('Ctrl Pts',(-1.5155908782104,1.04048605981312,3.88891791044777));
#25583=CARTESIAN_POINT('Ctrl Pts',(-1.69630815727945,-0.708636427490783,
4.00002985074626));
#25584=CARTESIAN_POINT('Ctrl Pts',(-0.325039216866852,-1.80941329116195,
4.11114179104478));
#25585=CARTESIAN_POINT('Ctrl Pts',(1.34361459616473,-1.25472178898058,4.22225373134328));
#25586=CARTESIAN_POINT('Ctrl Pts',(1.78296857449566,0.447939743012656,4.3333656716418));
#25587=CARTESIAN_POINT('Ctrl Pts',(0.591048986302979,1.74077225568864,4.44447761194029));
#25588=CARTESIAN_POINT('Ctrl Pts',(-1.14163312622272,1.44093745732314,4.55558955223881));
#25589=CARTESIAN_POINT('Ctrl Pts',(-1.82981228635293,-0.177239806233389,
4.66670149253731));
#25590=CARTESIAN_POINT('Ctrl Pts',(-0.843859631129698,-1.63325682938675,
4.77781343283583));
#25591=CARTESIAN_POINT('Ctrl Pts',(0.914157055608714,-1.59497455450745,
4.88892537313433));
#25592=CARTESIAN_POINT('Ctrl Pts',(1.83579319504673,-0.0974181938582904,
5.00003731343284));
#25593=CARTESIAN_POINT('Ctrl Pts',(1.07782545884778,1.48926801121999,5.11114925373134));
#25594=CARTESIAN_POINT('Ctrl Pts',(-0.666266304296033,1.713393176152,5.22226119402985));
#25595=CARTESIAN_POINT('Ctrl Pts',(-1.80077774751939,0.369900670398456,
5.33337313432836));
#25596=CARTESIAN_POINT('Ctrl Pts',(-1.28772159609117,-1.31202129819493,
5.44448507462686));
#25597=CARTESIAN_POINT('Ctrl Pts',(0.403496653242899,-1.79354886637635,
5.55559701492538));
#25598=CARTESIAN_POINT('Ctrl Pts',(1.72554797232085,-0.634122566945669,
5.66670895522387));
#25599=CARTESIAN_POINT('Ctrl Pts',(1.46886056527041,1.10547479200108,5.77782089552239));
#25600=CARTESIAN_POINT('Ctrl Pts',(-0.131715923640121,1.83365183655613,
5.88893283582089));
#25601=CARTESIAN_POINT('Ctrl Pts',(-1.61178439161985,0.884182935474394,
6.0000447761194));
#25602=CARTESIAN_POINT('Ctrl Pts',(-1.61719624754958,-0.874240214284601,
6.11115671641792));
#25603=CARTESIAN_POINT('Ctrl Pts',(-0.143008426055117,-1.83280806515592,
6.2222686567164));
#25604=CARTESIAN_POINT('Ctrl Pts',(1.4620310918033,-1.11449456034272,6.33338059701493));
#25605=CARTESIAN_POINT('Ctrl Pts',(1.72940928754233,0.623475815429911,6.44449253731343));
#25606=CARTESIAN_POINT('Ctrl Pts',(0.414554230167772,1.79104708014026,6.55560447761194));
#25607=CARTESIAN_POINT('Ctrl Pts',(-1.27965688051538,1.3198938381471,6.66671641791045));
#25608=CARTESIAN_POINT('Ctrl Pts',(-1.80294698305189,-0.358742811224428,
6.77782835820896));
#25609=CARTESIAN_POINT('Ctrl Pts',(-0.676946582872774,-1.70937536089767,
6.88894029850746));
#25610=CARTESIAN_POINT('Ctrl Pts',(1.06890459630572,-1.49565296874813,7.00005223880597));
#25611=CARTESIAN_POINT('Ctrl Pts',(1.83584092749207,0.0856835708872964,
7.11116417910447));
#25612=CARTESIAN_POINT('Ctrl Pts',(0.924965623038614,1.59014055343882,7.22227611940298));
#25613=CARTESIAN_POINT('Ctrl Pts',(-0.835858495286665,1.63675999125994,
7.33338805970149));
#25614=CARTESIAN_POINT('Ctrl Pts',(-1.49427628245053,0.673892957891604,
7.40746268656716));
#25615=CARTESIAN_POINT('Ctrl Pts',(-1.54730100999696,0.159498697368912,
7.4445));
#25616=CARTESIAN_POINT('',(0.903606778650208,-1.26612599672284,0.));
#25617=CARTESIAN_POINT('Ctrl Pts',(0.903606778650207,-1.26612599672284,
-1.38777878078145E-15));
#25618=CARTESIAN_POINT('Ctrl Pts',(1.32452548910467,-0.965725403881512,
0.0370373134328344));
#25619=CARTESIAN_POINT('Ctrl Pts',(1.83597806077316,0.082627195836251,0.111111940298506));
#25620=CARTESIAN_POINT('Ctrl Pts',(0.924927935979477,1.59016247494986,0.222223880597014));
#25621=CARTESIAN_POINT('Ctrl Pts',(-0.833133967250649,1.63815181774712,
0.333335820895521));
#25622=CARTESIAN_POINT('Ctrl Pts',(-1.5310648992002,0.622568787117098,0.411242452161949));
#25623=CARTESIAN_POINT('Ctrl Pts',(-1.55772948793458,0.0543297678623362,
0.452111769995541));
#25624=CARTESIAN_POINT('Ctrl Pts',(-1.55735958542387,0.00101297198046621,
0.455943774396298));
#25625=CARTESIAN_POINT('Ctrl Pts',(0.863568564283469,1.75641400930303,0.));
#25626=CARTESIAN_POINT('Ctrl Pts',(0.902603531943078,1.7324423702308,2.28859211685802E-17));
#25627=CARTESIAN_POINT('Ctrl Pts',(0.940676776691071,1.70703651305647,-1.38032481715684E-16));
#25628=CARTESIAN_POINT('Ctrl Pts',(0.977697814042708,1.68019172043607,-1.28369537222284E-16));
#25629=CARTESIAN_POINT('Ctrl Pts',(1.03585714935899,1.63801906923031,-1.20927094907836E-16));
#25630=CARTESIAN_POINT('Ctrl Pts',(1.09142188330105,1.59229630788867,-2.7046412047637E-16));
#25631=CARTESIAN_POINT('Ctrl Pts',(1.14423064795477,1.54336420856895,-1.97758476261356E-16));
#25632=CARTESIAN_POINT('Ctrl Pts',(1.16946834979149,1.51997919396061,-1.63011907532148E-16));
#25633=CARTESIAN_POINT('Ctrl Pts',(1.19407597424497,1.49586072902399,-7.62289135782024E-17));
#25634=CARTESIAN_POINT('Ctrl Pts',(1.21803226410959,1.47104407323701,-6.59194920871187E-17));
#25635=CARTESIAN_POINT('Ctrl Pts',(1.23017793652576,1.45846220127952,-6.0692687062697E-17));
#25636=CARTESIAN_POINT('Ctrl Pts',(1.24215614940632,1.44570084965787,-2.95883426371776E-16));
#25637=CARTESIAN_POINT('Ctrl Pts',(1.25396388375076,1.43276453675822,-3.36536354339501E-16));
#25638=CARTESIAN_POINT('Ctrl Pts',(1.2638543668245,1.42192872524363,-3.70588365016071E-16));
#25639=CARTESIAN_POINT('Ctrl Pts',(1.2736185550329,1.41097745381189,1.09305947039191E-16));
#25640=CARTESIAN_POINT('Ctrl Pts',(1.28325381741352,1.39991535359824,9.71445146547012E-17));
#25641=CARTESIAN_POINT('Ctrl Pts',(1.33014189367208,1.34608385655041,3.79633375853411E-17));
#25642=CARTESIAN_POINT('Ctrl Pts',(1.37399192615748,1.28961736627304,-2.11573378166283E-16));
#25643=CARTESIAN_POINT('Ctrl Pts',(1.4146405205773,1.23085017638072,-2.98372437868011E-16));
#25644=CARTESIAN_POINT('Ctrl Pts',(1.44368223570237,1.18886348503472,-3.60386723994296E-16));
#25645=CARTESIAN_POINT('Ctrl Pts',(1.47108885988106,1.14570172941536,-3.55315850605615E-16));
#25646=CARTESIAN_POINT('Ctrl Pts',(1.49678522627473,1.10148200990233,-3.88578058618805E-16));
#25647=CARTESIAN_POINT('Ctrl Pts',(1.51163132719121,1.07593402353214,-4.0779533196023E-16));
#25648=CARTESIAN_POINT('Ctrl Pts',(1.52590630204136,1.05003284136309,-4.46468072791598E-16));
#25649=CARTESIAN_POINT('Ctrl Pts',(1.53959352057452,1.02380089191946,-4.5102810375397E-16));
#25650=CARTESIAN_POINT('Ctrl Pts',(1.54536419749809,1.0127412230066,-4.5295066131244E-16));
#25651=CARTESIAN_POINT('Ctrl Pts',(1.55102598614157,1.00163115224642,-3.28801907372083E-16));
#25652=CARTESIAN_POINT('Ctrl Pts',(1.55657733146951,0.990474109820403,-3.19189119579733E-16));
#25653=CARTESIAN_POINT('Ctrl Pts',(1.58759135376405,0.928142415050821,-2.65484801564386E-16));
#25654=CARTESIAN_POINT('Ctrl Pts',(1.61517084797965,0.864329379202861,-6.67259587666608E-16));
#25655=CARTESIAN_POINT('Ctrl Pts',(1.6391617363075,0.799343273084874,-5.82867087928207E-16));
#25656=CARTESIAN_POINT('Ctrl Pts',(1.66256147081466,0.735958474279834,-5.00554083870677E-16));
#25657=CARTESIAN_POINT('Ctrl Pts',(1.68254736306605,0.671456731546573,9.30631015772363E-17));
#25658=CARTESIAN_POINT('Ctrl Pts',(1.69892809919455,0.606119085630755,1.11022302462516E-16));
#25659=CARTESIAN_POINT('Ctrl Pts',(1.70969727271493,0.563164212250211,1.2282920473501E-16));
#25660=CARTESIAN_POINT('Ctrl Pts',(1.71890726464806,0.519847981128071,-1.31890518419189E-16));
#25661=CARTESIAN_POINT('Ctrl Pts',(1.72649157325935,0.476251973430995,-1.38777878078145E-16));
#25662=CARTESIAN_POINT('Ctrl Pts',(1.73286785345701,0.439599936333954,-1.44568219328534E-16));
#25663=CARTESIAN_POINT('Ctrl Pts',(1.73809492661148,0.402750145627894,-3.72078883249312E-16));
#25664=CARTESIAN_POINT('Ctrl Pts',(1.74212769993621,0.365752815321986,-4.16333634234434E-16));
#25665=CARTESIAN_POINT('Ctrl Pts',(1.74338298809393,0.354236593888137,-4.30108885249319E-16));
#25666=CARTESIAN_POINT('Ctrl Pts',(1.7445224615788,0.34270569873049,-4.2222380310258E-18));
#25667=CARTESIAN_POINT('Ctrl Pts',(1.74554359854572,0.331176868161872,-1.38777878078145E-17));
#25668=CARTESIAN_POINT('Ctrl Pts',(1.75129265664821,0.266268908759598,-6.82390718242887E-17));
#25669=CARTESIAN_POINT('Ctrl Pts',(1.75330855751176,0.201308359017101,-1.61972025925174E-16));
#25670=CARTESIAN_POINT('Ctrl Pts',(1.75142416657778,0.13655560768634,-1.38777878078145E-16));
#25671=CARTESIAN_POINT('Ctrl Pts',(1.75088156113035,0.117910222074166,-1.32099183788468E-16));
#25672=CARTESIAN_POINT('Ctrl Pts',(1.75001524326664,0.0992821075343112,
-1.58618989379829E-17));
#25673=CARTESIAN_POINT('Ctrl Pts',(1.74882042289714,0.0806776277944099,
0.));
#25674=CARTESIAN_POINT('Ctrl Pts',(1.74441970791246,0.0121543460832101,
6.07280452025807E-17));
#25675=CARTESIAN_POINT('Ctrl Pts',(1.735566761163,-0.0560504444942819,-6.11382253507945E-17));
#25676=CARTESIAN_POINT('Ctrl Pts',(1.72245455146386,-0.123599567095003,
-1.38777878078145E-16));
#25677=CARTESIAN_POINT('Ctrl Pts',(1.7106535204694,-0.184393995170097,-2.08653815792513E-16));
#25678=CARTESIAN_POINT('Ctrl Pts',(1.69540126258663,-0.244657625690558,
-3.30909447568271E-16));
#25679=CARTESIAN_POINT('Ctrl Pts',(1.67680583516799,-0.304119468797943,
-3.05311331771918E-16));
#25680=CARTESIAN_POINT('Ctrl Pts',(1.673496966793,-0.314700102829495,-3.00756405772578E-16));
#25681=CARTESIAN_POINT('Ctrl Pts',(1.67008375904048,-0.325250056291554,
1.12130257435328E-16));
#25682=CARTESIAN_POINT('Ctrl Pts',(1.66656954022458,-0.335760782955591,
1.11022302462516E-16));
#25683=CARTESIAN_POINT('Ctrl Pts',(1.64601748634937,-0.397230211008769,
1.04542697325368E-16));
#25684=CARTESIAN_POINT('Ctrl Pts',(1.62199078115275,-0.457436083404927,
4.89063387979405E-18));
#25685=CARTESIAN_POINT('Ctrl Pts',(1.59467603738004,-0.516104439016194,
-1.11022302462516E-16));
#25686=CARTESIAN_POINT('Ctrl Pts',(1.56746949320957,-0.574540396593861,
-2.26476082617573E-16));
#25687=CARTESIAN_POINT('Ctrl Pts',(1.53700015167997,-0.631451830043097,
-2.65447621135955E-16));
#25688=CARTESIAN_POINT('Ctrl Pts',(1.50341281573621,-0.68653552753498,-3.60822483003176E-16));
#25689=CARTESIAN_POINT('Ctrl Pts',(1.4705131167318,-0.740491490894733,-4.54244725638714E-16));
#25690=CARTESIAN_POINT('Ctrl Pts',(1.43462103920338,-0.792694411910378,
-4.2831431104574E-16));
#25691=CARTESIAN_POINT('Ctrl Pts',(1.39584581076301,-0.842817530414533,
-5.27355936696949E-16));
#25692=CARTESIAN_POINT('Ctrl Pts',(1.38890062306969,-0.851795284506205,
-5.45095682077361E-16));
#25693=CARTESIAN_POINT('Ctrl Pts',(1.38186288427344,-0.860706190744767,
2.35960662867998E-16));
#25694=CARTESIAN_POINT('Ctrl Pts',(1.37473315631241,-0.86954820289757,2.4980018054066E-16));
#25695=CARTESIAN_POINT('Ctrl Pts',(1.36794195322354,-0.877970389630667,
2.62982587454478E-16));
#25696=CARTESIAN_POINT('Ctrl Pts',(1.36107048536455,-0.886326025058287,
-6.35152333120316E-18));
#25697=CARTESIAN_POINT('Ctrl Pts',(1.35412452302825,-0.894607674989563,
0.));
#25698=CARTESIAN_POINT('Ctrl Pts',(1.31424959800426,-0.942150427756674,
3.64624085702422E-17));
#25699=CARTESIAN_POINT('Ctrl Pts',(1.2718724912058,-0.987319961554271,-3.18360401148313E-16));
#25700=CARTESIAN_POINT('Ctrl Pts',(1.22713193424969,-1.02984905091596,-2.22044604925031E-16));
#25701=CARTESIAN_POINT('Ctrl Pts',(1.18319618732353,-1.0716131109617,-1.27461373607439E-16));
#25702=CARTESIAN_POINT('Ctrl Pts',(1.13698054744349,-1.11083140282356,-2.10671899724563E-16));
#25703=CARTESIAN_POINT('Ctrl Pts',(1.08859303083371,-1.14720695088303,-2.77555756156289E-16));
#25704=CARTESIAN_POINT('Ctrl Pts',(1.04174975410163,-1.18242160919609,-3.42305080264122E-16));
#25705=CARTESIAN_POINT('Ctrl Pts',(0.992870408249348,-1.21497237243561,
-3.26158703430296E-16));
#25706=CARTESIAN_POINT('Ctrl Pts',(0.942040458977608,-1.24454244204819,
-3.60822483003176E-16));
#25707=CARTESIAN_POINT('Ctrl Pts',(0.92935042596986,-1.25192480549339,-3.69476524828035E-16));
#25708=CARTESIAN_POINT('Ctrl Pts',(0.916538776387811,-1.25912113789668,
-6.13893683198417E-17));
#25709=CARTESIAN_POINT('Ctrl Pts',(0.903606778650223,-1.26612599672282,
-5.55111512312578E-17));
#25710=CARTESIAN_POINT('Ctrl Pts',(0.0849160311154397,1.9485495525967,7.04599999999999));
#25711=CARTESIAN_POINT('Ctrl Pts',(0.400605874250757,1.93520776532856,7.0280673457103));
#25712=CARTESIAN_POINT('Ctrl Pts',(0.713151734000586,1.84952766933244,7.01013469142061));
#25713=CARTESIAN_POINT('Ctrl Pts',(0.983981247423036,1.69229543406338,6.99220203713092));
#25714=CARTESIAN_POINT('Ctrl Pts',(1.54334058226818,1.36755490846516,6.95516472369808));
#25715=CARTESIAN_POINT('Ctrl Pts',(1.92475070653735,0.737594779052165,6.91812741026524));
#25716=CARTESIAN_POINT('Ctrl Pts',(1.95488643500235,0.0915387903718514,
6.88109009683241));
#25717=CARTESIAN_POINT('Ctrl Pts',(1.98502216346735,-0.554517198308454,
6.84405278339957));
#25718=CARTESIAN_POINT('Ctrl Pts',(1.6638834961282,-1.21666904625608,6.80701546996674));
#25719=CARTESIAN_POINT('Ctrl Pts',(1.13779469346529,-1.59249087768303,6.7699781565339));
#25720=CARTESIAN_POINT('Ctrl Pts',(0.611705890802371,-1.96831270910999,
6.73294084310107));
#25721=CARTESIAN_POINT('Ctrl Pts',(-0.119333047184302,-2.05780452401628,
6.69590352966823));
#25722=CARTESIAN_POINT('Ctrl Pts',(-0.720597162266781,-1.81977576072458,
6.65886621623539));
#25723=CARTESIAN_POINT('Ctrl Pts',(-1.32186127734926,-1.58174699743288,
6.62182890280256));
#25724=CARTESIAN_POINT('Ctrl Pts',(-1.79335056952755,-1.0161976559432,6.58479158936972));
#25725=CARTESIAN_POINT('Ctrl Pts',(-1.91953678206301,-0.381975860707627,
6.54775427593688));
#25726=CARTESIAN_POINT('Ctrl Pts',(-1.94439039128642,-0.257059672615188,
6.540459414666));
#25727=CARTESIAN_POINT('Ctrl Pts',(-1.9558486040335,-0.129479463263859,
6.53316455339512));
#25728=CARTESIAN_POINT('Ctrl Pts',(-1.95467666345581,-0.00169153748172557,
6.52586969212423));
#25729=CARTESIAN_POINT('Origin',(0.,0.,-1.2940562256037));
#25730=CARTESIAN_POINT('',(-0.903606778650191,-1.26612599672285,1.38777878078145E-16));
#25731=CARTESIAN_POINT('Ctrl Pts',(-0.905552056217056,-1.26793026328003,
8.26433105977076E-16));
#25732=CARTESIAN_POINT('Ctrl Pts',(-0.513280080436939,-1.54506079646518,
0.0345343505799217));
#25733=CARTESIAN_POINT('Ctrl Pts',(0.58913651448779,-1.72157402054048,0.106143938272268));
#25734=CARTESIAN_POINT('Ctrl Pts',(1.77597071143275,-0.477272995959146,
0.214828763077039));
#25735=CARTESIAN_POINT('Ctrl Pts',(1.3630442868689,1.23477489449879,0.326054474414316));
#25736=CARTESIAN_POINT('Ctrl Pts',(-0.299513989741265,1.81437004394786,
0.437280185751592));
#25737=CARTESIAN_POINT('Ctrl Pts',(-1.41424275662139,0.944368549815884,
0.526614102814722));
#25738=CARTESIAN_POINT('Ctrl Pts',(-1.55418552513067,0.213449522874851,
0.578872782765425));
#25739=CARTESIAN_POINT('Ctrl Pts',(-1.55327638232574,0.000749985450955847,
0.594056225603703));
#25740=CARTESIAN_POINT('Origin',(0.,0.,0.));
#25741=CARTESIAN_POINT('Ctrl Pts',(-0.685825729128727,1.39614588036675,
-0.230074082272066));
#25742=CARTESIAN_POINT('Ctrl Pts',(-1.15044430012221,1.1679123019855,-0.19299884515964));
#25743=CARTESIAN_POINT('Ctrl Pts',(-1.8258407957124,0.215070471435756,-0.118848370934789));
#25744=CARTESIAN_POINT('Ctrl Pts',(-1.16856980438922,-1.42158824274557,
-0.0076226595975132));
#25745=CARTESIAN_POINT('Ctrl Pts',(0.561390129169046,-1.75066389321976,
0.103603051739764));
#25746=CARTESIAN_POINT('Ctrl Pts',(1.77597071143275,-0.477272995959146,
0.214828763077039));
#25747=CARTESIAN_POINT('Ctrl Pts',(1.3630442868689,1.23477489449879,0.326054474414316));
#25748=CARTESIAN_POINT('Ctrl Pts',(-0.299513989741265,1.81437004394786,
0.437280185751592));
#25749=CARTESIAN_POINT('Ctrl Pts',(-1.68741350339127,0.731169639996686,
0.548505897088869));
#25750=CARTESIAN_POINT('Ctrl Pts',(-1.52862817745114,-1.02241621535808,
0.659731608426144));
#25751=CARTESIAN_POINT('Ctrl Pts',(0.0313843551128396,-1.83872969125081,
0.770957319763422));
#25752=CARTESIAN_POINT('Ctrl Pts',(1.56261245507102,-0.969643437172017,
0.882183031100698));
#25753=CARTESIAN_POINT('Ctrl Pts',(1.66150197094076,0.788277540412492,0.993408742437974));
#25754=CARTESIAN_POINT('Ctrl Pts',(0.237394066880885,1.82362194812979,1.10463445377525));
#25755=CARTESIAN_POINT('Ctrl Pts',(-1.40431546877471,1.18737513564603,1.21586016511253));
#25756=CARTESIAN_POINT('Ctrl Pts',(-1.75877981175223,-0.537266275957094,
1.3270858764498));
#25757=CARTESIAN_POINT('Ctrl Pts',(-0.501082205369057,-1.76942810040879,
1.43831158778708));
#25758=CARTESIAN_POINT('Ctrl Pts',(1.21592516185098,-1.37966899434435,1.54953729912436));
#25759=CARTESIAN_POINT('Ctrl Pts',(1.8183716526183,0.274745208061178,1.66076301046163));
#25760=CARTESIAN_POINT('Ctrl Pts',(0.754032712405612,1.67731773070425,1.77198872179891));
#25761=CARTESIAN_POINT('Ctrl Pts',(-1.00147988107901,1.54240019271928,1.88321443313619));
#25762=CARTESIAN_POINT('Ctrl Pts',(-1.83899975790172,-0.00633731701985082,
1.99444014447346));
#25763=CARTESIAN_POINT('Ctrl Pts',(-0.990825815880477,-1.5492657736205,
2.10566585581074));
#25764=CARTESIAN_POINT('Ctrl Pts',(0.765574959497512,-1.6720811124538,2.21689156714802));
#25765=CARTESIAN_POINT('Ctrl Pts',(1.82022199392772,-0.262206313316451,
2.32811727848529));
#25766=CARTESIAN_POINT('Ctrl Pts',(1.20638759997596,1.38801628675575,2.43934298982257));
#25767=CARTESIAN_POINT('Ctrl Pts',(-0.513265374585843,1.76593287340023,
2.55056870115984));
#25768=CARTESIAN_POINT('Ctrl Pts',(-1.76244071170529,0.525131406868061,
2.66179441249712));
#25769=CARTESIAN_POINT('Ctrl Pts',(-1.39609903883734,-1.19702453193727,
2.77302012383439));
#25770=CARTESIAN_POINT('Ctrl Pts',(0.249957593646744,-1.82194441691009,
2.88424583517168));
#25771=CARTESIAN_POINT('Ctrl Pts',(1.6668940398915,-0.776804039943688,2.99547154650895));
#25772=CARTESIAN_POINT('Ctrl Pts',(1.55589501744036,0.980383063583733,3.10669725784622));
#25773=CARTESIAN_POINT('Ctrl Pts',(0.0187062518377651,1.83891553174339,
3.2179229691835));
#25774=CARTESIAN_POINT('Ctrl Pts',(-1.53562934193987,1.01183139943408,3.32914868052078));
#25775=CARTESIAN_POINT('Ctrl Pts',(-1.68235144492823,-0.742734052303713,
3.44037439185806));
#25776=CARTESIAN_POINT('Ctrl Pts',(-0.286969261786828,-1.81648256240041,
3.55160010319533));
#25777=CARTESIAN_POINT('Ctrl Pts',(1.37145934362907,-1.22517734450477,3.66282581453261));
#25778=CARTESIAN_POINT('Ctrl Pts',(1.77275862659963,0.489169815626649,3.77405152586988));
#25779=CARTESIAN_POINT('Ctrl Pts',(0.549083125265984,1.75512620009375,3.88527723720716));
#25780=CARTESIAN_POINT('Ctrl Pts',(-1.17790186202284,1.41227032121617,3.99650294854444));
#25781=CARTESIAN_POINT('Ctrl Pts',(-1.82517932708368,-0.225123700760077,
4.10772865988171));
#25782=CARTESIAN_POINT('Ctrl Pts',(-0.799431294618187,-1.65616118233816,
4.21895437121899));
#25783=CARTESIAN_POINT('Ctrl Pts',(0.959104426053338,-1.56910132141185,
4.33018008255627));
#25784=CARTESIAN_POINT('Ctrl Pts',(1.83849028118038,-0.0437463405035559,
4.44140579389354));
#25785=CARTESIAN_POINT('Ctrl Pts',(1.0326493363287,1.52170812080878,4.55263150523082));
#25786=CARTESIAN_POINT('Ctrl Pts',(-0.719755403894915,1.69230978744094,
4.6638572165681));
#25787=CARTESIAN_POINT('Ctrl Pts',(-1.81240626272056,0.311678989548955,
4.77508292790537));
#25788=CARTESIAN_POINT('Ctrl Pts',(-1.24373988019232,-1.35464806069341,
4.88630863924265));
#25789=CARTESIAN_POINT('Ctrl Pts',(0.464983542380115,-1.77925562259896,
4.99753435057992));
#25790=CARTESIAN_POINT('Ctrl Pts',(1.74748619395055,-0.572933012383953,
5.1087600619172));
#25791=CARTESIAN_POINT('Ctrl Pts',(1.42817970701863,1.15856074316792,5.21998577325448));
#25792=CARTESIAN_POINT('Ctrl Pts',(-0.20024807751692,1.82807576816643,5.33121148459175));
#25793=CARTESIAN_POINT('Ctrl Pts',(-1.64512115233065,0.821910272029074,
5.44243719592903));
#25794=CARTESIAN_POINT('Ctrl Pts',(-1.58201670345687,-0.937647879740503,
5.55366290726631));
#25795=CARTESIAN_POINT('Ctrl Pts',(-0.0687781849042931,-1.83772416168987,
5.66488861860358));
#25796=CARTESIAN_POINT('Ctrl Pts',(1.50750444735784,-1.05327561457109,5.77611432994086));
#25797=CARTESIAN_POINT('Ctrl Pts',(1.70195476716013,0.696642984640571,5.88734004127814));
#25798=CARTESIAN_POINT('Ctrl Pts',(0.336330007005007,1.80799440678846,5.99856575261541));
#25799=CARTESIAN_POINT('Ctrl Pts',(-1.33758382509627,1.26207070464844,6.10979146395269));
#25800=CARTESIAN_POINT('Ctrl Pts',(-1.78542595464098,-0.440709020390059,
6.22101717528996));
#25801=CARTESIAN_POINT('Ctrl Pts',(-0.59667036110871,-1.73952595846347,
6.33224288662724));
#25802=CARTESIAN_POINT('Ctrl Pts',(1.13899278941852,-1.44381691390763,6.44346859796452));
#25803=CARTESIAN_POINT('Ctrl Pts',(1.83065601360088,0.17532136832598,6.5546943093018));
#25804=CARTESIAN_POINT('Ctrl Pts',(0.844193344579619,1.63380261073593,6.66592002063907));
#25805=CARTESIAN_POINT('Ctrl Pts',(-0.915934603694247,1.5945880622222,6.77714573197635));
#25806=CARTESIAN_POINT('Ctrl Pts',(-1.83677508915277,0.093893769326276,
6.88837144331362));
#25807=CARTESIAN_POINT('Ctrl Pts',(-1.07340561084952,-1.49320523543669,
6.99959715465089));
#25808=CARTESIAN_POINT('Ctrl Pts',(0.672826183539381,-1.71093187207897,
7.11082286598819));
#25809=CARTESIAN_POINT('Ctrl Pts',(1.80435891657647,-0.361603954366771,
7.22204857732544));
#25810=CARTESIAN_POINT('Ctrl Pts',(1.27791236939833,1.32169962363241,7.33327428866273));
#25811=CARTESIAN_POINT('Ctrl Pts',(0.152038852759137,1.63230677878407,7.40742476288758));
#25812=CARTESIAN_POINT('Ctrl Pts',(-0.352169241380528,1.51510959188617,
7.44450000000001));
#25813=CARTESIAN_POINT('Ctrl Pts',(-0.744392439309327,1.51537102412035,
-0.153382721514711));
#25814=CARTESIAN_POINT('Ctrl Pts',(-1.24868753458029,1.26764723230613,-0.116307484402285));
#25815=CARTESIAN_POINT('Ctrl Pts',(-1.9817601264938,0.233436609412224,-0.042157010177434));
#25816=CARTESIAN_POINT('Ctrl Pts',(-1.26836088272398,-1.54298606011064,
0.0690687011598421));
#25817=CARTESIAN_POINT('Ctrl Pts',(0.609330548428412,-1.9001634242276,0.180294412497119));
#25818=CARTESIAN_POINT('Ctrl Pts',(1.92763134113508,-0.518030156334108,
0.291520123834394));
#25819=CARTESIAN_POINT('Ctrl Pts',(1.47944269002272,1.34021961655124,0.402745835171672));
#25820=CARTESIAN_POINT('Ctrl Pts',(-0.325091258553406,1.96930981947839,
0.513971546508948));
#25821=CARTESIAN_POINT('Ctrl Pts',(-1.8315117099918,0.793608534572646,0.625197257846224));
#25822=CARTESIAN_POINT('Ctrl Pts',(-1.65916676712527,-1.10972637539669,
0.7364229691835));
#25823=CARTESIAN_POINT('Ctrl Pts',(0.0340644505831978,-1.9957496809569,
0.847648680520777));
#25824=CARTESIAN_POINT('Ctrl Pts',(1.69605316295611,-1.05244701795271,0.958874391858054));
#25825=CARTESIAN_POINT('Ctrl Pts',(1.80338743872602,0.855593215941119,1.07010010319533));
#25826=CARTESIAN_POINT('Ctrl Pts',(0.257666548537818,1.97935179840939,1.18132581453261));
#25827=CARTESIAN_POINT('Ctrl Pts',(-1.52423826194019,1.28877211229984,1.29255152586988));
#25828=CARTESIAN_POINT('Ctrl Pts',(-1.90897240898426,-0.583146616891169,
1.40377723720716));
#25829=CARTESIAN_POINT('Ctrl Pts',(-0.543872574776452,-1.9205300179086,
1.51500294854444));
#25830=CARTESIAN_POINT('Ctrl Pts',(1.31976019388731,-1.49748707947159,1.62622865988171));
#25831=CARTESIAN_POINT('Ctrl Pts',(1.97365314915069,0.298207324296545,1.73745437121899));
#25832=CARTESIAN_POINT('Ctrl Pts',(0.818424019786662,1.82055379963935,1.84868008255626));
#25833=CARTESIAN_POINT('Ctrl Pts',(-1.08700216386266,1.6741148561284,1.95990579389354));
#25834=CARTESIAN_POINT('Ctrl Pts',(-1.99604281019441,-0.00687849795467773,
2.07113150523082));
#25835=CARTESIAN_POINT('Ctrl Pts',(-1.07543828510332,-1.68156672953773,
2.1823572165681));
#25836=CARTESIAN_POINT('Ctrl Pts',(0.830951927537738,-1.81486999562381,
2.29358292790537));
#25837=CARTESIAN_POINT('Ctrl Pts',(1.97566150203448,-0.284597659262374,
2.40480863924265));
#25838=CARTESIAN_POINT('Ctrl Pts',(1.30940816326546,1.50654719648941,2.51603435057992));
#25839=CARTESIAN_POINT('Ctrl Pts',(-0.557096136778581,1.91673631281949,
2.6272600619172));
#25840=CARTESIAN_POINT('Ctrl Pts',(-1.91294593480924,0.569975479650009,
2.73848577325448));
#25841=CARTESIAN_POINT('Ctrl Pts',(-1.51532018251605,-1.29924552753932,
2.84971148459175));
#25842=CARTESIAN_POINT('Ctrl Pts',(0.271302949066904,-1.97753101288966,
2.96093719592903));
#25843=CARTESIAN_POINT('Ctrl Pts',(1.80923996829539,-0.843139925493371,
3.0721629072663));
#25844=CARTESIAN_POINT('Ctrl Pts',(1.6887620836463,1.06410376450264,3.18338861860358));
#25845=CARTESIAN_POINT('Ctrl Pts',(0.0203036891799667,1.9959513914669,3.29461432994085));
#25846=CARTESIAN_POINT('Ctrl Pts',(-1.66676580240553,1.09823765951648,3.40584004127814));
#25847=CARTESIAN_POINT('Ctrl Pts',(-1.82601737245506,-0.806160500357498,
3.51706575261541));
#25848=CARTESIAN_POINT('Ctrl Pts',(-0.31147526217729,-1.97160273836024,
3.6282914639527));
#25849=CARTESIAN_POINT('Ctrl Pts',(1.48857635818734,-1.32980247507055,3.73951717528996));
#25850=CARTESIAN_POINT('Ctrl Pts',(1.92414495740429,0.530942915707476,3.85074288662724));
#25851=CARTESIAN_POINT('Ctrl Pts',(0.595972576764652,1.90500679384439,3.96196859796451));
#25852=CARTESIAN_POINT('Ctrl Pts',(-1.27848985988335,1.53287242622092,4.07319430930179));
#25853=CARTESIAN_POINT('Ctrl Pts',(-1.98104217115158,-0.244348343372923,
4.18442002063907));
#25854=CARTESIAN_POINT('Ctrl Pts',(-0.867699455103643,-1.79759056863662,
4.29564573197634));
#25855=CARTESIAN_POINT('Ctrl Pts',(1.04100801842068,-1.70309615192351,4.40687144331362));
#25856=CARTESIAN_POINT('Ctrl Pts',(1.99548982624636,-0.047482098928651,
4.5180971546509));
#25857=CARTESIAN_POINT('Ctrl Pts',(1.12083336301401,1.65165576596945,4.62932286598818));
#25858=CARTESIAN_POINT('Ctrl Pts',(-0.781219569426276,1.83682611665882,
4.74054857732545));
#25859=CARTESIAN_POINT('Ctrl Pts',(-1.96717833937204,0.338295099553305,
4.85177428866273));
#25860=CARTESIAN_POINT('Ctrl Pts',(-1.34995017532929,-1.47032946049761,
4.963));
#25861=CARTESIAN_POINT('Ctrl Pts',(0.504691233720185,-1.93119677026974,
5.07422571133729));
#25862=CARTESIAN_POINT('Ctrl Pts',(1.89671436244713,-0.621859146624829,
5.18545142267455));
#25863=CARTESIAN_POINT('Ctrl Pts',(1.55014040845374,1.25749708864148,5.29667713401184));
#25864=CARTESIAN_POINT('Ctrl Pts',(-0.217348443720809,1.98418595644765,
5.4079028453491));
#25865=CARTESIAN_POINT('Ctrl Pts',(-1.78560776525334,0.892098045178891,
5.5191285566864));
#25866=CARTESIAN_POINT('Ctrl Pts',(-1.71711445473246,-1.01771917087445,
5.63035426802365));
#25867=CARTESIAN_POINT('Ctrl Pts',(-0.0746515603857894,-1.99465828328709,
5.74157997936095));
#25868=CARTESIAN_POINT('Ctrl Pts',(1.63623915694148,-1.14322104099488,5.85280569069821));
#25869=CARTESIAN_POINT('Ctrl Pts',(1.84729473816909,0.756133444166813,5.96403140203549));
#25870=CARTESIAN_POINT('Ctrl Pts',(0.365051213003408,1.96238972900109,6.07525711337277));
#25871=CARTESIAN_POINT('Ctrl Pts',(-1.45180800902444,1.36984637716583,6.18648282471005));
#25872=CARTESIAN_POINT('Ctrl Pts',(-1.93789402341296,-0.478343766907873,
6.29770853604731));
#25873=CARTESIAN_POINT('Ctrl Pts',(-0.647623567773631,-1.88807435543072,
6.4089342473846));
#25874=CARTESIAN_POINT('Ctrl Pts',(1.23625811173359,-1.56711296880792,6.52015995872187));
#25875=CARTESIAN_POINT('Ctrl Pts',(1.98698654428125,0.190293095590063,6.63138567005915));
#25876=CARTESIAN_POINT('Ctrl Pts',(0.916284000920563,1.77332266653327,6.74261138139642));
#25877=CARTESIAN_POINT('Ctrl Pts',(-0.994151669926352,1.73075935608174,
6.8538370927337));
#25878=CARTESIAN_POINT('Ctrl Pts',(-1.99362816383988,0.101911912919242,
6.96506280407097));
#25879=CARTESIAN_POINT('Ctrl Pts',(-1.16507005656334,-1.62071885084899,
7.07628851540826));
#25880=CARTESIAN_POINT('Ctrl Pts',(0.730282785733831,-1.85703845110468,
7.18751422674552));
#25881=CARTESIAN_POINT('Ctrl Pts',(1.95844378280506,-0.392483452023516,
7.29873993808281));
#25882=CARTESIAN_POINT('Ctrl Pts',(1.38704085524538,1.43456736176966,7.40996564942008));
#25883=CARTESIAN_POINT('Ctrl Pts',(0.165022348489246,1.77169909665516,7.48411612364493));
#25884=CARTESIAN_POINT('Ctrl Pts',(-0.382243053164543,1.64449374968465,
7.52119136075736));
#25885=CARTESIAN_POINT('Ctrl Pts',(-0.802959149489926,1.63459616787395,
-0.0766913607573553));
#25886=CARTESIAN_POINT('Ctrl Pts',(-1.34693076903838,1.36738216262677,-0.0396161236449298));
#25887=CARTESIAN_POINT('Ctrl Pts',(-2.1376794572752,0.251802747388692,0.034534350579921));
#25888=CARTESIAN_POINT('Ctrl Pts',(-1.36815196105874,-1.66438387747571,
0.145760061917198));
#25889=CARTESIAN_POINT('Ctrl Pts',(0.657270967687777,-2.04966295523545,
0.256985773254474));
#25890=CARTESIAN_POINT('Ctrl Pts',(2.07929197083741,-0.558787316709069,
0.36821148459175));
#25891=CARTESIAN_POINT('Ctrl Pts',(1.59584109317654,1.44566433860368,0.479437195929027));
#25892=CARTESIAN_POINT('Ctrl Pts',(-0.350668527365547,2.12424959500892,
0.590662907266303));
#25893=CARTESIAN_POINT('Ctrl Pts',(-1.97560991659234,0.856047429148608,
0.70188861860358));
#25894=CARTESIAN_POINT('Ctrl Pts',(-1.7897053567994,-1.1970365354353,0.813114329940855));
#25895=CARTESIAN_POINT('Ctrl Pts',(0.0367445460535571,-2.15276967066298,
0.924340041278132));
#25896=CARTESIAN_POINT('Ctrl Pts',(1.8294938708412,-1.13525059873339,1.03556575261541));
#25897=CARTESIAN_POINT('Ctrl Pts',(1.94527290651128,0.922908891469747,1.14679146395268));
#25898=CARTESIAN_POINT('Ctrl Pts',(0.277939030194749,2.13508164868898,1.25801717528996));
#25899=CARTESIAN_POINT('Ctrl Pts',(-1.64416105510567,1.39016908895364,1.36924288662724));
#25900=CARTESIAN_POINT('Ctrl Pts',(-2.05916500621629,-0.629026957825243,
1.48046859796451));
#25901=CARTESIAN_POINT('Ctrl Pts',(-0.586662944183848,-2.07163193540842,
1.59169430930179));
#25902=CARTESIAN_POINT('Ctrl Pts',(1.42359522592366,-1.61530516459883,1.70292002063907));
#25903=CARTESIAN_POINT('Ctrl Pts',(2.12893464568308,0.32166944053191,1.81414573197634));
#25904=CARTESIAN_POINT('Ctrl Pts',(0.882815327167714,1.96378986857444,1.92537144331362));
#25905=CARTESIAN_POINT('Ctrl Pts',(-1.17252444664632,1.80582951953752,2.0365971546509));
#25906=CARTESIAN_POINT('Ctrl Pts',(-2.1530858624871,-0.00741967888950297,
2.14782286598817));
#25907=CARTESIAN_POINT('Ctrl Pts',(-1.16005075432617,-1.81386768545496,
2.25904857732545));
#25908=CARTESIAN_POINT('Ctrl Pts',(0.896328895577965,-1.95765887879382,
2.37027428866273));
#25909=CARTESIAN_POINT('Ctrl Pts',(2.13110101014124,-0.306989005208296,
2.4815));
#25910=CARTESIAN_POINT('Ctrl Pts',(1.41242872655496,1.62507810622307,2.59272571133728));
#25911=CARTESIAN_POINT('Ctrl Pts',(-0.600926898971321,2.06753975223876,
2.70395142267456));
#25912=CARTESIAN_POINT('Ctrl Pts',(-2.06345115791318,0.614819552431958,
2.81517713401183));
#25913=CARTESIAN_POINT('Ctrl Pts',(-1.63454132619476,-1.40146652314137,
2.92640284534911));
#25914=CARTESIAN_POINT('Ctrl Pts',(0.292648304487066,-2.13311760886924,
3.03762855668638));
#25915=CARTESIAN_POINT('Ctrl Pts',(1.95158589669928,-0.909475811043054,
3.14885426802366));
#25916=CARTESIAN_POINT('Ctrl Pts',(1.82162914985223,1.14782446542155,3.26007997936093));
#25917=CARTESIAN_POINT('Ctrl Pts',(0.021901126522171,2.15298725119041,3.37130569069822));
#25918=CARTESIAN_POINT('Ctrl Pts',(-1.79790226287119,1.18464391959888,3.48253140203548));
#25919=CARTESIAN_POINT('Ctrl Pts',(-1.96968329998188,-0.869586948411284,
3.59375711337277));
#25920=CARTESIAN_POINT('Ctrl Pts',(-0.335981262567754,-2.12672291432008,
3.70498282471004));
#25921=CARTESIAN_POINT('Ctrl Pts',(1.60569337274561,-1.43442760563632,3.81620853604732));
#25922=CARTESIAN_POINT('Ctrl Pts',(2.07553128820896,0.572716015788303,3.9274342473846));
#25923=CARTESIAN_POINT('Ctrl Pts',(0.642862028263319,2.05488738759502,4.03865995872187));
#25924=CARTESIAN_POINT('Ctrl Pts',(-1.37907785774386,1.65347453122567,4.14988567005915));
#25925=CARTESIAN_POINT('Ctrl Pts',(-2.13690501521948,-0.263572985985768,
4.26111138139642));
#25926=CARTESIAN_POINT('Ctrl Pts',(-0.935967615589101,-1.93901995493508,
4.3723370927337));
#25927=CARTESIAN_POINT('Ctrl Pts',(1.12291161078803,-1.83709098243517,4.48356280407097));
#25928=CARTESIAN_POINT('Ctrl Pts',(2.15248937131234,-0.0512178573537473,
4.59478851540826));
#25929=CARTESIAN_POINT('Ctrl Pts',(1.20901738969933,1.78160341113012,4.70601422674553));
#25930=CARTESIAN_POINT('Ctrl Pts',(-0.842683734957634,1.9813424458767,4.81723993808281));
#25931=CARTESIAN_POINT('Ctrl Pts',(-2.12195041602352,0.364911209557656,
4.92846564942008));
#25932=CARTESIAN_POINT('Ctrl Pts',(-1.45616047046626,-1.58601086030181,
5.03969136075736));
#25933=CARTESIAN_POINT('Ctrl Pts',(0.544398925060255,-2.08313791794051,
5.15091707209464));
#25934=CARTESIAN_POINT('Ctrl Pts',(2.04594253094371,-0.670785280865706,
5.26214278343191));
#25935=CARTESIAN_POINT('Ctrl Pts',(1.67210110988885,1.35643343411504,5.37336849476919));
#25936=CARTESIAN_POINT('Ctrl Pts',(-0.234448809924699,2.14029614472887,
5.48459420610646));
#25937=CARTESIAN_POINT('Ctrl Pts',(-1.92609437817603,0.96228581832871,5.59581991744374));
#25938=CARTESIAN_POINT('Ctrl Pts',(-1.85221220600806,-1.09779046200839,
5.70704562878101));
#25939=CARTESIAN_POINT('Ctrl Pts',(-0.0805249358672843,-2.15159240488431,
5.8182713401183));
#25940=CARTESIAN_POINT('Ctrl Pts',(1.76497386652513,-1.23316646741867,5.92949705145556));
#25941=CARTESIAN_POINT('Ctrl Pts',(1.99263470917806,0.815623903693059,6.04072276279285));
#25942=CARTESIAN_POINT('Ctrl Pts',(0.393772419001808,2.11678505121371,6.15194847413012));
#25943=CARTESIAN_POINT('Ctrl Pts',(-1.56603219295262,1.47762204968323,6.2631741854674));
#25944=CARTESIAN_POINT('Ctrl Pts',(-2.09036209218494,-0.515978513425692,
6.37439989680467));
#25945=CARTESIAN_POINT('Ctrl Pts',(-0.698576774438554,-2.03662275239797,
6.48562560814195));
#25946=CARTESIAN_POINT('Ctrl Pts',(1.33352343404865,-1.69040902370822,6.59685131947923));
#25947=CARTESIAN_POINT('Ctrl Pts',(2.14331707496162,0.205264822854154,6.70807703081651));
#25948=CARTESIAN_POINT('Ctrl Pts',(0.988374657261507,1.9128427223306,6.81930274215378));
#25949=CARTESIAN_POINT('Ctrl Pts',(-1.07236873615846,1.86693064994129,6.93052845349106));
#25950=CARTESIAN_POINT('Ctrl Pts',(-2.15048123852699,0.109930056512203,
7.04175416482834));
#25951=CARTESIAN_POINT('Ctrl Pts',(-1.25673450227717,-1.74823246626129,
7.1529798761656));
#25952=CARTESIAN_POINT('Ctrl Pts',(0.787739387928281,-2.00314503013039,
7.26420558750289));
#25953=CARTESIAN_POINT('Ctrl Pts',(2.11252864903365,-0.42336294968026,7.37543129884016));
#25954=CARTESIAN_POINT('Ctrl Pts',(1.49616934109244,1.54743509990691,7.48665701017744));
#25955=CARTESIAN_POINT('Ctrl Pts',(0.178005844219355,1.91109141452625,7.56080748440229));
#25956=CARTESIAN_POINT('Ctrl Pts',(-0.412316864948557,1.77387790748314,
7.59788272151472));
#25957=CARTESIAN_POINT('Ctrl Pts',(-0.861525859670525,1.75382131162755,
0.));
#25958=CARTESIAN_POINT('Ctrl Pts',(-1.44517400349647,1.4671170929474,0.0370752371124254));
#25959=CARTESIAN_POINT('Ctrl Pts',(-2.29359878805659,0.270168885365161,
0.111225711337276));
#25960=CARTESIAN_POINT('Ctrl Pts',(-1.46794303939349,-1.78578169484077,
0.222451422674553));
#25961=CARTESIAN_POINT('Ctrl Pts',(0.705211386947141,-2.19916248624329,
0.33367713401183));
#25962=CARTESIAN_POINT('Ctrl Pts',(2.23095260053975,-0.599544477084032,
0.444902845349104));
#25963=CARTESIAN_POINT('Ctrl Pts',(1.71223949633035,1.55110906065613,0.556128556686383));
#25964=CARTESIAN_POINT('Ctrl Pts',(-0.376245796177686,2.27918937053945,
0.667354268023658));
#25965=CARTESIAN_POINT('Ctrl Pts',(-2.11970812319287,0.918486323724569,
0.778579979360935));
#25966=CARTESIAN_POINT('Ctrl Pts',(-1.92024394647352,-1.28434669547391,
0.889805690698211));
#25967=CARTESIAN_POINT('Ctrl Pts',(0.0394246415239131,-2.30978966036907,
1.00103140203549));
#25968=CARTESIAN_POINT('Ctrl Pts',(1.96293457872629,-1.21805417951409,1.11225711337277));
#25969=CARTESIAN_POINT('Ctrl Pts',(2.08715837429654,0.990224566998375,1.22348282471004));
#25970=CARTESIAN_POINT('Ctrl Pts',(0.298211511851683,2.29081149896857,1.33470853604732));
#25971=CARTESIAN_POINT('Ctrl Pts',(-1.76408384827114,1.49156606560744,1.44593424738459));
#25972=CARTESIAN_POINT('Ctrl Pts',(-2.20935760344832,-0.674907298759319,
1.55715995872187));
#25973=CARTESIAN_POINT('Ctrl Pts',(-0.629453313591242,-2.22273385290824,
1.66838567005915));
#25974=CARTESIAN_POINT('Ctrl Pts',(1.52743025795999,-1.73312324972607,1.77961138139642));
#25975=CARTESIAN_POINT('Ctrl Pts',(2.28421614221547,0.345131556767278,1.8908370927337));
#25976=CARTESIAN_POINT('Ctrl Pts',(0.947206634548765,2.10702593750954,2.00206280407097));
#25977=CARTESIAN_POINT('Ctrl Pts',(-1.25804672942998,1.93754418294664,2.11328851540825));
#25978=CARTESIAN_POINT('Ctrl Pts',(-2.31012891477979,-0.0079608598243287,
2.22451422674552));
#25979=CARTESIAN_POINT('Ctrl Pts',(-1.24466322354901,-1.94616864137219,
2.33573993808281));
#25980=CARTESIAN_POINT('Ctrl Pts',(0.961705863618192,-2.10044776196383,
2.44696564942008));
#25981=CARTESIAN_POINT('Ctrl Pts',(2.286540518248,-0.329380351154219,2.55819136075736));
#25982=CARTESIAN_POINT('Ctrl Pts',(1.51544928984446,1.74360901595674,2.66941707209463));
#25983=CARTESIAN_POINT('Ctrl Pts',(-0.644757661164061,2.21834319165802,
2.78064278343191));
#25984=CARTESIAN_POINT('Ctrl Pts',(-2.21395638101712,0.659663625213907,
2.89186849476918));
#25985=CARTESIAN_POINT('Ctrl Pts',(-1.75376246987347,-1.50368751874342,
3.00309420610647));
#25986=CARTESIAN_POINT('Ctrl Pts',(0.313993659907229,-2.28870420484881,
3.11431991744373));
#25987=CARTESIAN_POINT('Ctrl Pts',(2.09393182510317,-0.975811696592738,
3.22554562878102));
#25988=CARTESIAN_POINT('Ctrl Pts',(1.95449621605817,1.23154516634045,3.33677134011829));
#25989=CARTESIAN_POINT('Ctrl Pts',(0.0234985638643735,2.31002311091391,
3.44799705145557));
#25990=CARTESIAN_POINT('Ctrl Pts',(-1.92903872333685,1.27105017968128,3.55922276279284));
#25991=CARTESIAN_POINT('Ctrl Pts',(-2.1133492275087,-0.93301339646507,3.67044847413012));
#25992=CARTESIAN_POINT('Ctrl Pts',(-0.360487262958215,-2.28184309027991,
3.7816741854674));
#25993=CARTESIAN_POINT('Ctrl Pts',(1.72281038730387,-1.53905273620209,3.89289989680467));
#25994=CARTESIAN_POINT('Ctrl Pts',(2.22691761901362,0.614489115869131,4.00412560814195));
#25995=CARTESIAN_POINT('Ctrl Pts',(0.689751479761988,2.20476798134566,4.11535131947922));
#25996=CARTESIAN_POINT('Ctrl Pts',(-1.47966585560437,1.77407663623043,4.22657703081651));
#25997=CARTESIAN_POINT('Ctrl Pts',(-2.29276785928738,-0.282797628598616,
4.33780274215377));
#25998=CARTESIAN_POINT('Ctrl Pts',(-1.00423577607456,-2.08044934123353,
4.44902845349105));
#25999=CARTESIAN_POINT('Ctrl Pts',(1.20481520315537,-1.97108581294683,4.56025416482834));
#26000=CARTESIAN_POINT('Ctrl Pts',(2.30948891637831,-0.0549536157788429,
4.6714798761656));
#26001=CARTESIAN_POINT('Ctrl Pts',(1.29720141638464,1.91155105629079,4.78270558750289));
#26002=CARTESIAN_POINT('Ctrl Pts',(-0.904147900488994,2.12585877509457,
4.89393129884016));
#26003=CARTESIAN_POINT('Ctrl Pts',(-2.276722492675,0.391527319562006,5.00515701017744));
#26004=CARTESIAN_POINT('Ctrl Pts',(-1.56237076560323,-1.701692260106,5.11638272151471));
#26005=CARTESIAN_POINT('Ctrl Pts',(0.584106616400323,-2.2350790656113,5.227608432852));
#26006=CARTESIAN_POINT('Ctrl Pts',(2.19517069944029,-0.71971141510658,5.33883414418926));
#26007=CARTESIAN_POINT('Ctrl Pts',(1.79406181132396,1.4553697795886,5.45005985552654));
#26008=CARTESIAN_POINT('Ctrl Pts',(-0.251549176128587,2.2964063330101,5.56128556686382));
#26009=CARTESIAN_POINT('Ctrl Pts',(-2.06658099109872,1.03247359147853,5.6725112782011));
#26010=CARTESIAN_POINT('Ctrl Pts',(-1.98730995728366,-1.17786175314234,
5.78373698953836));
#26011=CARTESIAN_POINT('Ctrl Pts',(-0.0863983113487825,-2.30852652648153,
5.89496270087566));
#26012=CARTESIAN_POINT('Ctrl Pts',(1.89370857610877,-1.32311189384246,6.00618841221292));
#26013=CARTESIAN_POINT('Ctrl Pts',(2.13797468018702,0.875114363219305,6.1174141235502));
#26014=CARTESIAN_POINT('Ctrl Pts',(0.422493625000208,2.27118037342633,6.22863983488748));
#26015=CARTESIAN_POINT('Ctrl Pts',(-1.68025637688079,1.58539772220062,6.33986554622475));
#26016=CARTESIAN_POINT('Ctrl Pts',(-2.24283016095692,-0.55361325994351,
6.45109125756204));
#26017=CARTESIAN_POINT('Ctrl Pts',(-0.749529981103475,-2.18517114936522,
6.56231696889931));
#26018=CARTESIAN_POINT('Ctrl Pts',(1.43078875636371,-1.81370507860851,6.67354268023658));
#26019=CARTESIAN_POINT('Ctrl Pts',(2.29964760564199,0.22023655011824,6.78476839157387));
#26020=CARTESIAN_POINT('Ctrl Pts',(1.06046531360245,2.05236277812793,6.89599410291113));
#26021=CARTESIAN_POINT('Ctrl Pts',(-1.15058580239056,2.00310194380083,7.00721981424842));
#26022=CARTESIAN_POINT('Ctrl Pts',(-2.30733431321409,0.117948200105168,
7.11844552558569));
#26023=CARTESIAN_POINT('Ctrl Pts',(-1.34839894799099,-1.87574608167359,
7.22967123692297));
#26024=CARTESIAN_POINT('Ctrl Pts',(0.845195990122731,-2.1492516091561,7.34089694826023));
#26025=CARTESIAN_POINT('Ctrl Pts',(2.26661351526224,-0.454242447337005,
7.45212265959753));
#26026=CARTESIAN_POINT('Ctrl Pts',(1.60529782693949,1.66030283804416,7.56334837093479));
#26027=CARTESIAN_POINT('Ctrl Pts',(0.190989339949464,2.05048373239734,7.63749884515964));
#26028=CARTESIAN_POINT('Ctrl Pts',(-0.442390676732572,1.90326206528163,
7.67457408227207));
#26029=CARTESIAN_POINT('Ctrl Pts',(-1.95381346134878,-0.0017935399644829,
6.42413030787577));
#26030=CARTESIAN_POINT('Ctrl Pts',(-1.9552538907035,-0.159408210813097,
6.43311729110453));
#26031=CARTESIAN_POINT('Ctrl Pts',(-1.93778561972322,-0.316707681574419,
6.44210427433328));
#26032=CARTESIAN_POINT('Ctrl Pts',(-1.90018450030199,-0.469037744489771,
6.45109125756203));
#26033=CARTESIAN_POINT('Ctrl Pts',(-1.7450634343391,-1.09746588975075,6.48816649467446));
#26034=CARTESIAN_POINT('Ctrl Pts',(-1.24729670772129,-1.64131851955799,
6.52524173178688));
#26035=CARTESIAN_POINT('Ctrl Pts',(-0.635026888167849,-1.85133382266882,
6.56231696889931));
#26036=CARTESIAN_POINT('Ctrl Pts',(-0.02275706861441,-2.06134912577965,
6.59939220601173));
#26037=CARTESIAN_POINT('Ctrl Pts',(0.704015843874659,-1.93752710219408,
6.63646744312416));
#26038=CARTESIAN_POINT('Ctrl Pts',(1.21221210833224,-1.53662581894683,6.67354268023658));
#26039=CARTESIAN_POINT('Ctrl Pts',(1.7204083727898,-1.1357245356996,6.71061791734901));
#26040=CARTESIAN_POINT('Ctrl Pts',(2.01002798921589,-0.457743992790703,
6.74769315446144));
#26041=CARTESIAN_POINT('Ctrl Pts',(1.94830741542236,0.186600649998693,6.78476839157386));
#26042=CARTESIAN_POINT('Ctrl Pts',(1.88658684162883,0.830945292788112,6.82184362868628));
#26043=CARTESIAN_POINT('Ctrl Pts',(1.47352607761564,1.44165403545803,6.85891886579871));
#26044=CARTESIAN_POINT('Ctrl Pts',(0.898487176276873,1.73879826773846,6.89599410291113));
#26045=CARTESIAN_POINT('Ctrl Pts',(0.323448274938114,2.0359425000189,6.93306934002356));
#26046=CARTESIAN_POINT('Ctrl Pts',(-0.413568763726226,2.01952222190986,
6.97014457713599));
#26047=CARTESIAN_POINT('Ctrl Pts',(-0.974868701528982,1.69711979223941,
7.00721981424841));
#26048=CARTESIAN_POINT('Ctrl Pts',(-1.17057269468519,1.58471029663753,7.02014654283228));
#26049=CARTESIAN_POINT('Ctrl Pts',(-1.344915597571,1.43510400955329,7.03307327141614));
#26050=CARTESIAN_POINT('Ctrl Pts',(-1.49039960333529,1.260503289177,7.046));
#26051=CARTESIAN_POINT('Ctrl Pts',(-0.905552056217064,-1.26793026328003,
2.94902990916057E-17));
#26052=CARTESIAN_POINT('Ctrl Pts',(-0.937134822631023,-1.25104249355971,
4.75162406228688E-17));
#26053=CARTESIAN_POINT('Ctrl Pts',(-0.968036761240596,-1.23301924856148,
-1.58634398933136E-16));
#26054=CARTESIAN_POINT('Ctrl Pts',(-0.998189477963827,-1.21387418528302,
-1.99493199737333E-16));
#26055=CARTESIAN_POINT('Ctrl Pts',(-1.04824220989901,-1.18209387411058,
-2.7512401071258E-16));
#26056=CARTESIAN_POINT('Ctrl Pts',(-1.09623172292828,-1.14722531738451,
-1.13947733410607E-16));
#26057=CARTESIAN_POINT('Ctrl Pts',(-1.14207949782356,-1.10958932626875,
-2.28983498828939E-16));
#26058=CARTESIAN_POINT('Ctrl Pts',(-1.16812476791348,-1.08820901815237,
-2.94333182366767E-16));
#26059=CARTESIAN_POINT('Ctrl Pts',(-1.19347860393222,-1.06593466358557,
-2.59231987339497E-16));
#26060=CARTESIAN_POINT('Ctrl Pts',(-1.21812392229353,-1.04281835170969,
-2.1163626406917E-16));
#26061=CARTESIAN_POINT('Ctrl Pts',(-1.23207453972119,-1.02973323677667,
-1.84694444255666E-16));
#26062=CARTESIAN_POINT('Ctrl Pts',(-1.24580226168736,-1.01637377846959,
3.24804729171387E-17));
#26063=CARTESIAN_POINT('Ctrl Pts',(-1.2592797890629,-1.00277371885107,1.38777878078145E-17));
#26064=CARTESIAN_POINT('Ctrl Pts',(-1.30315654392119,-0.95849805423447,
-4.66841707402696E-17));
#26065=CARTESIAN_POINT('Ctrl Pts',(-1.34442524303116,-0.911639949761556,
-4.44200463634023E-16));
#26066=CARTESIAN_POINT('Ctrl Pts',(-1.38299703120573,-0.862548384977714,
-4.09394740330526E-16));
#26067=CARTESIAN_POINT('Ctrl Pts',(-1.41261207961662,-0.824856353147081,
-3.82671240347992E-16));
#26068=CARTESIAN_POINT('Ctrl Pts',(-1.44063702556457,-0.785846462927244,
-3.12176496943412E-16));
#26069=CARTESIAN_POINT('Ctrl Pts',(-1.46702161869435,-0.745658482546257,
-3.67761376907083E-16));
#26070=CARTESIAN_POINT('Ctrl Pts',(-1.48012065014873,-0.725706550124602,
-3.9535733366299E-16));
#26071=CARTESIAN_POINT('Ctrl Pts',(-1.4928152185087,-0.705464023789787,
-1.55640291167757E-16));
#26072=CARTESIAN_POINT('Ctrl Pts',(-1.50509817356396,-0.68494682789941,
-1.17961196366423E-16));
#26073=CARTESIAN_POINT('Ctrl Pts',(-1.5112932288107,-0.674598734832467,
-9.89572943826601E-17));
#26074=CARTESIAN_POINT('Ctrl Pts',(-1.51737856906155,-0.664189090325049,
-2.93080070452884E-16));
#26075=CARTESIAN_POINT('Ctrl Pts',(-1.52335311621856,-0.653721302282831,
-2.77555756156289E-16));
#26076=CARTESIAN_POINT('Ctrl Pts',(-1.55547318924941,-0.597444883744102,
-1.94094684403748E-16));
#26077=CARTESIAN_POINT('Ctrl Pts',(-1.58439860819566,-0.539482552118629,
-3.31420483543467E-16));
#26078=CARTESIAN_POINT('Ctrl Pts',(-1.61003533926912,-0.480187572841947,
-3.19189119579733E-16));
#26079=CARTESIAN_POINT('Ctrl Pts',(-1.63616747730804,-0.419746770969312,
-3.06721395415186E-16));
#26080=CARTESIAN_POINT('Ctrl Pts',(-1.65888335052524,-0.357920523309995,
-2.80209762252872E-16));
#26081=CARTESIAN_POINT('Ctrl Pts',(-1.67804895967927,-0.295042072125015,
-1.66533453693773E-16));
#26082=CARTESIAN_POINT('Ctrl Pts',(-1.69039160882678,-0.254548359888778,
-9.33259296514283E-17));
#26083=CARTESIAN_POINT('Ctrl Pts',(-1.70126111007635,-0.213617460141972,
-2.30505991696603E-16));
#26084=CARTESIAN_POINT('Ctrl Pts',(-1.71061208520917,-0.172332131165316,
-2.91433543964104E-16));
#26085=CARTESIAN_POINT('Ctrl Pts',(-1.715816487101,-0.149354266164202,-3.2534353343379E-16));
#26086=CARTESIAN_POINT('Ctrl Pts',(-1.72055036402814,-0.126266539334649,
-1.00298932279788E-16));
#26087=CARTESIAN_POINT('Ctrl Pts',(-1.72480472543126,-0.103082789841687,
-9.71445146547012E-17));
#26088=CARTESIAN_POINT('Ctrl Pts',(-1.72695538876364,-0.0913629486676286,
-9.55498945276206E-17));
#26089=CARTESIAN_POINT('Ctrl Pts',(-1.72898375858757,-0.07961694527504,
-1.96680959500023E-16));
#26090=CARTESIAN_POINT('Ctrl Pts',(-1.73088777000182,-0.0678516147389183,
-1.94289029309402E-16));
#26091=CARTESIAN_POINT('Ctrl Pts',(-1.74172080812434,-0.000911745960731708,
-1.80679934979654E-16));
#26092=CARTESIAN_POINT('Ctrl Pts',(-1.74848760095285,0.0663732156671881,
-2.27318435210151E-17));
#26093=CARTESIAN_POINT('Ctrl Pts',(-1.75106859893149,0.133645381706535,
-4.16333634234434E-17));
#26094=CARTESIAN_POINT('Ctrl Pts',(-1.75197360252239,0.157233758116401,
-4.82610103750263E-17));
#26095=CARTESIAN_POINT('Ctrl Pts',(-1.75236359562623,0.180820850215305,
-8.28170566717793E-17));
#26096=CARTESIAN_POINT('Ctrl Pts',(-1.75223214201128,0.204392038445102,
-5.55111512312578E-17));
#26097=CARTESIAN_POINT('Ctrl Pts',(-1.75187057279805,0.269225675666801,
2.10533692500149E-17));
#26098=CARTESIAN_POINT('Ctrl Pts',(-1.74756789056806,0.333938320850628,
-1.60420900056E-17));
#26099=CARTESIAN_POINT('Ctrl Pts',(-1.73954116331082,0.398294466418659,
0.));
#26100=CARTESIAN_POINT('Ctrl Pts',(-1.73091740426649,0.467437452671242,
1.72353082822116E-17));
#26101=CARTESIAN_POINT('Ctrl Pts',(-1.71799540177027,0.536169874708505,
-4.36478159584899E-17));
#26102=CARTESIAN_POINT('Ctrl Pts',(-1.70098034075862,0.604204029641736,
8.32667268468867E-17));
#26103=CARTESIAN_POINT('Ctrl Pts',(-1.69824130486499,0.615155973465351,
1.03697067233541E-16));
#26104=CARTESIAN_POINT('Ctrl Pts',(-1.69539827041295,0.626080961021427,
1.29813171089747E-16));
#26105=CARTESIAN_POINT('Ctrl Pts',(-1.69245305315959,0.636975805303662,
1.11022302462516E-16));
#26106=CARTESIAN_POINT('Ctrl Pts',(-1.67473398681781,0.702521553550295,
-2.02764230671151E-18));
#26107=CARTESIAN_POINT('Ctrl Pts',(-1.65331496860816,0.766998932259627,
-2.57263159617093E-16));
#26108=CARTESIAN_POINT('Ctrl Pts',(-1.62845169327078,0.83015154980978,-1.94289029309402E-16));
#26109=CARTESIAN_POINT('Ctrl Pts',(-1.60307671281799,0.894603896257815,
-1.30018843507023E-16));
#26110=CARTESIAN_POINT('Ctrl Pts',(-1.57411406965586,0.957677277748301,
-1.42237185085071E-16));
#26111=CARTESIAN_POINT('Ctrl Pts',(-1.54178048300264,1.01910167818773,-5.55111512312578E-17));
#26112=CARTESIAN_POINT('Ctrl Pts',(-1.50922784853364,1.08094220569947,3.18024186880875E-17));
#26113=CARTESIAN_POINT('Ctrl Pts',(-1.47325811155629,1.14111231916335,-1.86023089836484E-16));
#26114=CARTESIAN_POINT('Ctrl Pts',(-1.43404118681899,1.19932479720781,-1.66533453693773E-16));
#26115=CARTESIAN_POINT('Ctrl Pts',(-1.42513259519695,1.21254845504633,-1.62106150675484E-16));
#26116=CARTESIAN_POINT('Ctrl Pts',(-1.41605624454103,1.22567101155683,-3.77067070771252E-16));
#26117=CARTESIAN_POINT('Ctrl Pts',(-1.40681378949184,1.23868893327645,-3.88578058618805E-16));
#26118=CARTESIAN_POINT('Ctrl Pts',(-1.40005105796202,1.24821418486786,-3.97000682266051E-16));
#26119=CARTESIAN_POINT('Ctrl Pts',(-1.39319940015811,1.25768325768832,-4.06719094166719E-16));
#26120=CARTESIAN_POINT('Ctrl Pts',(-1.3862680939899,1.26708342641975,-3.88578058618805E-16));
#26121=CARTESIAN_POINT('Ctrl Pts',(-1.34342259960335,1.32519006127916,-2.76440228046676E-16));
#26122=CARTESIAN_POINT('Ctrl Pts',(-1.2974598126633,1.38077597290076,-1.69458509682717E-16));
#26123=CARTESIAN_POINT('Ctrl Pts',(-1.24862081372783,1.43356038861728,-1.94289029309402E-16));
#26124=CARTESIAN_POINT('Ctrl Pts',(-1.19966911793571,1.48646660530969,-2.19176845800727E-16));
#26125=CARTESIAN_POINT('Ctrl Pts',(-1.14782748930566,1.53655939185262,-1.74330404157582E-16));
#26126=CARTESIAN_POINT('Ctrl Pts',(-1.09328907277386,1.5835398262669,-5.55111512312578E-17));
#26127=CARTESIAN_POINT('Ctrl Pts',(-1.03991703070208,1.62951552342795,6.07669985463979E-17));
#26128=CARTESIAN_POINT('Ctrl Pts',(-0.983961746585148,1.67251142482066,
1.56834561468643E-16));
#26129=CARTESIAN_POINT('Ctrl Pts',(-0.925564466602708,1.71221823957964,
2.22044604925031E-16));
#26130=CARTESIAN_POINT('Ctrl Pts',(-0.904533489913129,1.72651810244765,
2.45529104618684E-16));
#26131=CARTESIAN_POINT('Ctrl Pts',(-0.883185451447723,1.74039103644132,
-1.04689938393391E-17));
#26132=CARTESIAN_POINT('Ctrl Pts',(-0.861525859670525,1.75382131162755,
0.));
#26133=CARTESIAN_POINT('Origin',(0.,0.,0.));
#26134=CARTESIAN_POINT('Origin',(-0.866025403784439,-1.5,-4.));
#26135=CARTESIAN_POINT('',(-0.866025403784439,-1.5,-4.));
#26136=CARTESIAN_POINT('',(0.866025403784439,-1.5,-4.));
#26137=CARTESIAN_POINT('',(-0.43301270189222,-1.5,-4.));
#26138=CARTESIAN_POINT('',(-0.866025403784439,-1.5,-2.));
#26139=CARTESIAN_POINT('',(-0.866025403784439,-1.5,-4.));
#26140=CARTESIAN_POINT('',(0.866025403784439,-1.5,-2.));
#26141=CARTESIAN_POINT('',(-0.866025403784439,-1.5,-2.));
#26142=CARTESIAN_POINT('',(0.866025403784439,-1.5,-4.));
#26143=CARTESIAN_POINT('Origin',(-1.73205080756888,2.12115047744981E-16,
-4.));
#26144=CARTESIAN_POINT('',(-1.73205080756888,2.12115047744981E-16,-4.));
#26145=CARTESIAN_POINT('',(-1.51554445662277,-0.375,-4.));
#26146=CARTESIAN_POINT('',(-1.73205080756888,2.77555756156289E-16,-2.));
#26147=CARTESIAN_POINT('',(-1.73205080756888,2.12115047744981E-16,-4.));
#26148=CARTESIAN_POINT('',(-1.73205080756888,2.12115047744981E-16,-2.));
#26149=CARTESIAN_POINT('Origin',(-0.866025403784438,1.5,-4.));
#26150=CARTESIAN_POINT('',(-0.866025403784438,1.5,-4.));
#26151=CARTESIAN_POINT('',(-1.08253175473055,1.125,-4.));
#26152=CARTESIAN_POINT('',(-0.866025403784438,1.5,-2.));
#26153=CARTESIAN_POINT('',(-0.866025403784438,1.5,-4.));
#26154=CARTESIAN_POINT('',(-0.866025403784438,1.5,-2.));
#26155=CARTESIAN_POINT('Origin',(0.866025403784439,1.5,-4.));
#26156=CARTESIAN_POINT('',(0.866025403784439,1.5,-4.));
#26157=CARTESIAN_POINT('',(0.43301270189222,1.5,-4.));
#26158=CARTESIAN_POINT('',(0.866025403784439,1.5,-2.));
#26159=CARTESIAN_POINT('',(0.866025403784439,1.5,-4.));
#26160=CARTESIAN_POINT('',(0.866025403784439,1.5,-2.));
#26161=CARTESIAN_POINT('Origin',(1.73205080756888,0.,-4.));
#26162=CARTESIAN_POINT('',(1.73205080756888,0.,-4.));
#26163=CARTESIAN_POINT('',(1.51554445662277,0.375,-4.));
#26164=CARTESIAN_POINT('',(1.73205080756888,0.,-2.));
#26165=CARTESIAN_POINT('',(1.73205080756888,0.,-4.));
#26166=CARTESIAN_POINT('',(1.73205080756888,0.,-2.));
#26167=CARTESIAN_POINT('Origin',(0.866025403784439,-1.5,-4.));
#26168=CARTESIAN_POINT('',(1.08253175473055,-1.125,-4.));
#26169=CARTESIAN_POINT('',(0.866025403784439,-1.5,-2.));
#26170=CARTESIAN_POINT('Origin',(0.,2.77555756156289E-16,-2.));
#26171=CARTESIAN_POINT('Origin',(0.,0.,0.));
#26172=CARTESIAN_POINT('',(-3.5,-4.28626379701574E-16,0.));
#26173=CARTESIAN_POINT('Origin',(0.,0.,0.));
#26174=CARTESIAN_POINT('Origin',(0.,0.,-4.));
#26175=CARTESIAN_POINT('',(-3.5,-4.28626379701574E-16,-4.));
#26176=CARTESIAN_POINT('',(-3.5,-4.28626379701574E-16,-4.));
#26177=CARTESIAN_POINT('Origin',(0.,0.,-4.));
#26178=CARTESIAN_POINT('Origin',(0.,0.,-4.));
#26179=CARTESIAN_POINT('Origin',(0.,0.,8.));
#26180=CARTESIAN_POINT('',(0.,0.,0.));
#26181=CARTESIAN_POINT('Origin',(-5.,-9.,0.));
#26182=CARTESIAN_POINT('',(-5.,-9.,0.));
#26183=CARTESIAN_POINT('',(-5.,9.,0.));
#26184=CARTESIAN_POINT('',(-5.,-4.5,0.));
#26185=CARTESIAN_POINT('',(-5.,-9.,-3.));
#26186=CARTESIAN_POINT('',(-5.,-9.,0.));
#26187=CARTESIAN_POINT('',(-5.,9.,-3.));
#26188=CARTESIAN_POINT('',(-5.,-4.5,-3.));
#26189=CARTESIAN_POINT('',(-5.,9.,0.));
#26190=CARTESIAN_POINT('Origin',(-12.5,0.,0.));
#26191=CARTESIAN_POINT('',(0.,-9.,0.));
#26192=CARTESIAN_POINT('',(-6.25,-9.,0.));
#26193=CARTESIAN_POINT('',(0.,9.,0.));
#26194=CARTESIAN_POINT('',(-8.75,9.,0.));
#26195=CARTESIAN_POINT('',(0.,25.,0.));
#26196=CARTESIAN_POINT('',(0.,-25.,0.));
#26197=CARTESIAN_POINT('',(-25.,25.,0.));
#26198=CARTESIAN_POINT('',(0.,25.,0.));
#26199=CARTESIAN_POINT('',(-25.,-25.,0.));
#26200=CARTESIAN_POINT('',(-25.,25.,0.));
#26201=CARTESIAN_POINT('',(0.,-25.,0.));
#26202=CARTESIAN_POINT('',(-25.,-25.,0.));
#26203=CARTESIAN_POINT('',(0.,-25.,0.));
#26204=CARTESIAN_POINT('',(-18.5,15.,0.));
#26205=CARTESIAN_POINT('Origin',(-15.,15.,0.));
#26206=CARTESIAN_POINT('',(-18.5,-15.,0.));
#26207=CARTESIAN_POINT('Origin',(-15.,-15.,0.));
#26208=CARTESIAN_POINT('Origin',(-15.,-15.,-1.5));
#26209=CARTESIAN_POINT('',(-18.5,-15.,-3.));
#26210=CARTESIAN_POINT('',(-18.5,-15.,-1.5));
#26211=CARTESIAN_POINT('Origin',(-15.,-15.,-3.));
#26212=CARTESIAN_POINT('Origin',(-15.,15.,-1.5));
#26213=CARTESIAN_POINT('',(-18.5,15.,-3.));
#26214=CARTESIAN_POINT('',(-18.5,15.,-1.5));
#26215=CARTESIAN_POINT('Origin',(-15.,15.,-3.));
#26216=CARTESIAN_POINT('Origin',(0.,9.,-5.));
#26217=CARTESIAN_POINT('',(-4.58257569495584,25.,-3.));
#26218=CARTESIAN_POINT('',(-4.58257569495584,9.,-3.));
#26219=CARTESIAN_POINT('',(-4.58257569495584,9.,-3.));
#26220=CARTESIAN_POINT('Origin',(0.,25.,-5.));
#26221=CARTESIAN_POINT('Origin',(0.,9.,-5.));
#26222=CARTESIAN_POINT('Origin',(0.,9.,-5.));
#26223=CARTESIAN_POINT('',(-2.,25.,-5.));
#26224=CARTESIAN_POINT('Origin',(0.,25.,-5.));
#26225=CARTESIAN_POINT('',(-2.,9.,-5.));
#26226=CARTESIAN_POINT('',(-2.,9.,-5.));
#26227=CARTESIAN_POINT('Origin',(0.,9.,-5.));
#26228=CARTESIAN_POINT('Origin',(0.,9.,-5.));
#26229=CARTESIAN_POINT('',(-8.75,9.,-3.));
#26230=CARTESIAN_POINT('Origin',(0.,-9.,-5.));
#26231=CARTESIAN_POINT('',(-4.58257569495584,-9.,-3.));
#26232=CARTESIAN_POINT('',(-6.25,-9.,-3.));
#26233=CARTESIAN_POINT('Origin',(0.,-9.,-5.));
#26234=CARTESIAN_POINT('',(-2.,-9.,-5.));
#26235=CARTESIAN_POINT('Origin',(0.,-9.,-5.));
#26236=CARTESIAN_POINT('Origin',(0.,-25.,-5.));
#26237=CARTESIAN_POINT('',(-2.,-25.,-5.));
#26238=CARTESIAN_POINT('',(-2.,-25.,-5.));
#26239=CARTESIAN_POINT('Origin',(0.,-25.,-5.));
#26240=CARTESIAN_POINT('Origin',(0.,-25.,-5.));
#26241=CARTESIAN_POINT('',(-4.58257569495584,-25.,-3.));
#26242=CARTESIAN_POINT('',(-4.58257569495584,-25.,-3.));
#26243=CARTESIAN_POINT('Origin',(0.,-25.,-5.));
#26244=CARTESIAN_POINT('Origin',(-25.,-25.,-3.));
#26245=CARTESIAN_POINT('',(-25.,-25.,-3.));
#26246=CARTESIAN_POINT('',(-25.,-25.,-3.));
#26247=CARTESIAN_POINT('',(-25.,-25.,-3.));
#26248=CARTESIAN_POINT('Origin',(0.,25.,-3.));
#26249=CARTESIAN_POINT('',(-25.,25.,-3.));
#26250=CARTESIAN_POINT('',(0.,25.,-3.));
#26251=CARTESIAN_POINT('',(-25.,25.,-3.));
#26252=CARTESIAN_POINT('Origin',(-25.,25.,-3.));
#26253=CARTESIAN_POINT('',(-25.,25.,-3.));
#26254=CARTESIAN_POINT('Origin',(-12.5,0.,-3.));
#26255=CARTESIAN_POINT('',(0.,0.,0.));
#26256=CARTESIAN_POINT('Origin',(0.,0.,51.));
#26257=CARTESIAN_POINT('',(-1.5,-1.83697019872103E-16,50.));
#26258=CARTESIAN_POINT('Origin',(0.,0.,50.));
#26259=CARTESIAN_POINT('',(-1.5,-1.83697019872103E-16,52.));
#26260=CARTESIAN_POINT('',(-1.5,-1.83697019872103E-16,51.));
#26261=CARTESIAN_POINT('Origin',(0.,0.,52.));
#26262=CARTESIAN_POINT('Origin',(5.5,0.,50.));
#26263=CARTESIAN_POINT('',(-2.,2.44929359829471E-16,50.));
#26264=CARTESIAN_POINT('Origin',(0.,0.,50.));
#26265=CARTESIAN_POINT('Origin',(1.5,0.,52.));
#26266=CARTESIAN_POINT('',(-2.,-2.44929359829471E-16,52.));
#26267=CARTESIAN_POINT('Origin',(0.,0.,52.));
#26268=CARTESIAN_POINT('Origin',(0.,0.,0.));
#26269=CARTESIAN_POINT('',(-2.,-2.44929359829471E-16,53.));
#26270=CARTESIAN_POINT('Origin',(0.,0.,53.));
#26271=CARTESIAN_POINT('',(-2.,-2.44929359829471E-16,0.));
#26272=CARTESIAN_POINT('Origin',(0.,0.,0.));
#26273=CARTESIAN_POINT('',(-4.,-4.89858719658941E-16,0.));
#26274=CARTESIAN_POINT('Origin',(0.,0.,0.));
#26275=CARTESIAN_POINT('',(-2.,-2.44929359829471E-16,0.));
#26276=CARTESIAN_POINT('Origin',(0.,0.,0.));
#26277=CARTESIAN_POINT('Origin',(0.,0.,-2.));
#26278=CARTESIAN_POINT('',(-4.,-4.89858719658941E-16,-2.));
#26279=CARTESIAN_POINT('',(-4.,-4.89858719658941E-16,-2.));
#26280=CARTESIAN_POINT('Origin',(0.,0.,-2.));
#26281=CARTESIAN_POINT('Origin',(0.,0.,-2.));
#26282=CARTESIAN_POINT('Origin',(0.,0.,0.));
#26283=CARTESIAN_POINT('',(-2.,-2.44929359829471E-16,0.));
#26284=CARTESIAN_POINT('Origin',(0.,0.,53.));
#26285=CARTESIAN_POINT('',(0.,0.,0.));
#26286=CARTESIAN_POINT('Origin',(-1.,0.,1.));
#26287=CARTESIAN_POINT('',(-1.,1.11803398874989,0.));
#26288=CARTESIAN_POINT('',(-1.,1.11803398874989,1.));
#26289=CARTESIAN_POINT('',(-1.,1.11803398874989,0.));
#26290=CARTESIAN_POINT('',(-1.,3.87298334620742,0.));
#26291=CARTESIAN_POINT('',(-1.,0.,0.));
#26292=CARTESIAN_POINT('',(-1.,3.87298334620742,1.));
#26293=CARTESIAN_POINT('',(-1.,3.87298334620742,0.));
#26294=CARTESIAN_POINT('',(-1.,0.,1.));
#26295=CARTESIAN_POINT('Origin',(1.,8.,1.));
#26296=CARTESIAN_POINT('',(1.,1.11803398874989,1.));
#26297=CARTESIAN_POINT('',(1.,1.11803398874989,0.));
#26298=CARTESIAN_POINT('',(1.,1.11803398874989,0.));
#26299=CARTESIAN_POINT('',(1.,3.87298334620742,1.));
#26300=CARTESIAN_POINT('',(1.,4.,1.));
#26301=CARTESIAN_POINT('',(1.,3.87298334620742,0.));
#26302=CARTESIAN_POINT('',(1.,3.87298334620742,0.));
#26303=CARTESIAN_POINT('',(1.,4.,0.));
#26304=CARTESIAN_POINT('Origin',(0.,0.,0.));
#26305=CARTESIAN_POINT('Origin',(0.,0.,0.));
#26306=CARTESIAN_POINT('Origin',(0.,0.,0.));
#26307=CARTESIAN_POINT('Origin',(0.,0.,0.));
#26308=CARTESIAN_POINT('Origin',(0.,0.,1.));
#26309=CARTESIAN_POINT('Origin',(0.,0.,0.));
#26310=CARTESIAN_POINT('Origin',(0.,0.,1.));
#26311=CARTESIAN_POINT('Origin',(0.,0.,1.));
#26312=CARTESIAN_POINT('',(0.,0.,0.));
#26313=CARTESIAN_POINT('Origin',(5.,-9.,0.));
#26314=CARTESIAN_POINT('',(5.,-9.,0.));
#26315=CARTESIAN_POINT('',(5.,-25.,0.));
#26316=CARTESIAN_POINT('',(5.,-4.5,0.));
#26317=CARTESIAN_POINT('',(5.,-9.,-3.));
#26318=CARTESIAN_POINT('',(5.,-9.,0.));
#26319=CARTESIAN_POINT('',(5.,-25.,-3.));
#26320=CARTESIAN_POINT('',(5.,-4.5,-3.));
#26321=CARTESIAN_POINT('',(5.,-25.,-1.5));
#26322=CARTESIAN_POINT('Origin',(5.,25.,0.));
#26323=CARTESIAN_POINT('',(5.,25.,0.));
#26324=CARTESIAN_POINT('',(5.,9.,0.));
#26325=CARTESIAN_POINT('',(5.,12.5,0.));
#26326=CARTESIAN_POINT('',(5.,25.,-3.));
#26327=CARTESIAN_POINT('',(5.,25.,-1.5));
#26328=CARTESIAN_POINT('',(5.,9.,-3.));
#26329=CARTESIAN_POINT('',(5.,12.5,-3.));
#26330=CARTESIAN_POINT('',(5.,9.,0.));
#26331=CARTESIAN_POINT('Origin',(22.5,0.,-3.));
#26332=CARTESIAN_POINT('',(4.58257569495584,-9.,-3.));
#26333=CARTESIAN_POINT('',(11.25,-9.,-3.));
#26334=CARTESIAN_POINT('',(4.58257569495584,9.,-3.));
#26335=CARTESIAN_POINT('',(4.58257569495584,-9.,-3.));
#26336=CARTESIAN_POINT('',(13.75,9.,-3.));
#26337=CARTESIAN_POINT('',(45.,25.,-3.));
#26338=CARTESIAN_POINT('',(45.,25.,-3.));
#26339=CARTESIAN_POINT('',(45.,-25.,-3.));
#26340=CARTESIAN_POINT('',(45.,-25.,-3.));
#26341=CARTESIAN_POINT('',(0.,-25.,-3.));
#26342=CARTESIAN_POINT('',(26.5,15.,-3.));
#26343=CARTESIAN_POINT('Origin',(30.,15.,-3.));
#26344=CARTESIAN_POINT('',(26.5,-15.,-3.));
#26345=CARTESIAN_POINT('Origin',(30.,-15.,-3.));
#26346=CARTESIAN_POINT('Origin',(45.,25.,-3.));
#26347=CARTESIAN_POINT('',(45.,25.,0.));
#26348=CARTESIAN_POINT('',(45.,25.,0.));
#26349=CARTESIAN_POINT('',(45.,25.,-3.));
#26350=CARTESIAN_POINT('Origin',(30.,-15.,-1.5));
#26351=CARTESIAN_POINT('',(26.5,-15.,0.));
#26352=CARTESIAN_POINT('Origin',(30.,-15.,0.));
#26353=CARTESIAN_POINT('',(26.5,-15.,-1.5));
#26354=CARTESIAN_POINT('Origin',(30.,15.,-1.5));
#26355=CARTESIAN_POINT('',(26.5,15.,0.));
#26356=CARTESIAN_POINT('Origin',(30.,15.,0.));
#26357=CARTESIAN_POINT('',(26.5,15.,-1.5));
#26358=CARTESIAN_POINT('Origin',(0.,9.,-5.));
#26359=CARTESIAN_POINT('',(0.,9.,0.));
#26360=CARTESIAN_POINT('Origin',(0.,9.,-5.));
#26361=CARTESIAN_POINT('',(13.75,9.,0.));
#26362=CARTESIAN_POINT('',(-2.,9.,-5.));
#26363=CARTESIAN_POINT('Origin',(0.,9.,-5.));
#26364=CARTESIAN_POINT('Origin',(0.,-9.,-5.));
#26365=CARTESIAN_POINT('',(-2.,-9.,-5.));
#26366=CARTESIAN_POINT('',(-2.,-9.,-5.));
#26367=CARTESIAN_POINT('Origin',(0.,-9.,-5.));
#26368=CARTESIAN_POINT('Origin',(0.,-9.,-5.));
#26369=CARTESIAN_POINT('',(0.,-9.,0.));
#26370=CARTESIAN_POINT('',(0.,25.,0.));
#26371=CARTESIAN_POINT('Origin',(0.,-9.,-5.));
#26372=CARTESIAN_POINT('Origin',(0.,-9.,-5.));
#26373=CARTESIAN_POINT('',(11.25,-9.,0.));
#26374=CARTESIAN_POINT('Origin',(45.,-25.,-3.));
#26375=CARTESIAN_POINT('',(45.,-25.,0.));
#26376=CARTESIAN_POINT('',(45.,-25.,0.));
#26377=CARTESIAN_POINT('',(45.,-25.,-3.));
#26378=CARTESIAN_POINT('Origin',(0.,-25.,-3.));
#26379=CARTESIAN_POINT('',(0.,-25.,0.));
#26380=CARTESIAN_POINT('Origin',(22.5,0.,0.));
#26381=CARTESIAN_POINT('',(0.,0.,0.));
#26382=CARTESIAN_POINT('Origin',(0.,0.,0.));
#26383=CARTESIAN_POINT('',(-3.5,-4.28626379701574E-16,5.));
#26384=CARTESIAN_POINT('Origin',(0.,0.,5.));
#26385=CARTESIAN_POINT('',(-3.5,-4.28626379701574E-16,0.));
#26386=CARTESIAN_POINT('',(-3.5,-4.28626379701574E-16,0.));
#26387=CARTESIAN_POINT('Origin',(0.,0.,0.));
#26388=CARTESIAN_POINT('Origin',(0.,0.,0.));
#26389=CARTESIAN_POINT('',(-5.,-6.12323399573677E-16,5.));
#26390=CARTESIAN_POINT('Origin',(0.,0.,5.));
#26391=CARTESIAN_POINT('',(-5.,-6.12323399573677E-16,0.));
#26392=CARTESIAN_POINT('',(-5.,-6.12323399573677E-16,0.));
#26393=CARTESIAN_POINT('Origin',(0.,0.,0.));
#26394=CARTESIAN_POINT('Origin',(0.,0.,5.));
#26395=CARTESIAN_POINT('Origin',(0.,0.,0.));
#26396=CARTESIAN_POINT('',(0.,0.,0.));
#26397=CARTESIAN_POINT('Origin',(0.,0.,0.));
#26398=CARTESIAN_POINT('',(-2.94521004790112,0.00203952464144973,0.322176117089595));
#26399=CARTESIAN_POINT('',(-2.94462969622312,0.00314068971924443,0.177823882910389));
#26400=CARTESIAN_POINT('',(-2.942,-3.60291088309151E-16,0.));
#26401=CARTESIAN_POINT('',(1.28892185405323,2.64462557919717,0.));
#26402=CARTESIAN_POINT('Ctrl Pts',(-2.94521004790112,0.00203952464144973,
0.322176117089595));
#26403=CARTESIAN_POINT('Ctrl Pts',(-2.94603324667188,0.114074791781704,
0.316095866004171));
#26404=CARTESIAN_POINT('Ctrl Pts',(-2.94019223072851,0.226018346108296,
0.310015614918747));
#26405=CARTESIAN_POINT('Ctrl Pts',(-2.92739988843454,0.337155312555215,
0.303935363833323));
#26406=CARTESIAN_POINT('Ctrl Pts',(-2.81638858583978,1.30159631391204,0.251171250930097));
#26407=CARTESIAN_POINT('Ctrl Pts',(-2.18189506715083,2.20529575467607,0.198407138026871));
#26408=CARTESIAN_POINT('Ctrl Pts',(-1.31250721789878,2.63803669000119,0.145643025123645));
#26409=CARTESIAN_POINT('Ctrl Pts',(-0.512593100747222,3.03619682478308,
0.0970953500824302));
#26410=CARTESIAN_POINT('Ctrl Pts',(0.486174006333883,3.03566063209391,0.0485476750412151));
#26411=CARTESIAN_POINT('Ctrl Pts',(1.29201086331817,2.64828936846223,6.93889390390723E-17));
#26412=CARTESIAN_POINT('',(-1.28892185405326,2.64462557919716,0.));
#26413=CARTESIAN_POINT('Origin',(0.,0.,0.));
#26414=CARTESIAN_POINT('Ctrl Pts',(-1.28892185405326,2.64462557919716,1.59594559789866E-15));
#26415=CARTESIAN_POINT('Ctrl Pts',(-2.16624189914079,2.21704256404097,0.0527975766957825));
#26416=CARTESIAN_POINT('Ctrl Pts',(-2.80665150218763,1.32243360512987,0.105595153391563));
#26417=CARTESIAN_POINT('Ctrl Pts',(-2.92450934358977,0.359669350507257,
0.158392730087344));
#26418=CARTESIAN_POINT('Ctrl Pts',(-2.93896779585848,0.241560272181372,
0.164869781028359));
#26419=CARTESIAN_POINT('Ctrl Pts',(-2.94556202255218,0.122425479928277,
0.171346831969374));
#26420=CARTESIAN_POINT('Ctrl Pts',(-2.94462969622312,0.00314068971924443,
0.177823882910389));
#26421=CARTESIAN_POINT('Origin',(0.,0.,0.));
#26422=CARTESIAN_POINT('',(-2.93759410342513,0.00104371380931417,1.32217611708959));
#26423=CARTESIAN_POINT('',(-2.93753976560994,0.00101398507028504,1.17782388291039));
#26424=CARTESIAN_POINT('',(-2.942,-3.60291088309151E-16,0.));
#26425=CARTESIAN_POINT('Ctrl Pts',(-2.93759410342513,0.00104371380931417,
1.32217611708959));
#26426=CARTESIAN_POINT('Ctrl Pts',(-2.93894740988071,0.424518101105222,
1.29934721009019));
#26427=CARTESIAN_POINT('Ctrl Pts',(-2.85336411585787,0.847470416247501,
1.27651830309079));
#26428=CARTESIAN_POINT('Ctrl Pts',(-2.67811890996276,1.22926576308214,1.25368939609139));
#26429=CARTESIAN_POINT('Ctrl Pts',(-2.27307727438026,2.11170366459169,1.20092528318816));
#26430=CARTESIAN_POINT('Ctrl Pts',(-1.38905821992549,2.77427944140463,1.14816117028494));
#26431=CARTESIAN_POINT('Ctrl Pts',(-0.428414463428333,2.91544748851427,
1.09539705738171));
#26432=CARTESIAN_POINT('Ctrl Pts',(0.532229293068828,3.05661553562391,1.04263294447848));
#26433=CARTESIAN_POINT('Ctrl Pts',(1.56949775160839,2.67637585303025,0.989868831575259));
#26434=CARTESIAN_POINT('Ctrl Pts',(2.21127556875009,1.94774980228162,0.937104718672033));
#26435=CARTESIAN_POINT('Ctrl Pts',(2.8530533858918,1.21912375153298,0.884340605768807));
#26436=CARTESIAN_POINT('Ctrl Pts',(3.09934056163565,0.142111332629363,0.831576492865582));
#26437=CARTESIAN_POINT('Ctrl Pts',(2.83805568324674,-0.79300892305516,0.778812379962356));
#26438=CARTESIAN_POINT('Ctrl Pts',(2.57677080485782,-1.72812917873969,0.72604826705913));
#26439=CARTESIAN_POINT('Ctrl Pts',(1.80791387233614,-2.52135727120512,0.673284154155903));
#26440=CARTESIAN_POINT('Ctrl Pts',(0.881397688767813,-2.81181555894288,
0.620520041252678));
#26441=CARTESIAN_POINT('Ctrl Pts',(-0.0451184948005073,-3.10227384668064,
0.567755928349452));
#26442=CARTESIAN_POINT('Ctrl Pts',(-1.12929392941546,-2.88996232969074,
0.514991815446226));
#26443=CARTESIAN_POINT('Ctrl Pts',(-1.87761710347266,-2.27121529022098,
0.462227702543001));
#26444=CARTESIAN_POINT('Ctrl Pts',(-2.53970756099287,-1.72376931413192,
0.415543840725199));
#26445=CARTESIAN_POINT('Ctrl Pts',(-2.93888956917045,-0.858161617780837,
0.368859978907397));
#26446=CARTESIAN_POINT('Ctrl Pts',(-2.94521004790112,0.00203952464144973,
0.322176117089595));
#26447=CARTESIAN_POINT('Ctrl Pts',(-2.94462969622312,0.00314068971924443,
0.177823882910389));
#26448=CARTESIAN_POINT('Ctrl Pts',(-2.93796217945806,-0.849922571222733,
0.224144408665155));
#26449=CARTESIAN_POINT('Ctrl Pts',(-2.54635872365652,-1.71065728599598,
0.270464934419922));
#26450=CARTESIAN_POINT('Ctrl Pts',(-1.89332424994401,-2.25876726457989,
0.316785460174689));
#26451=CARTESIAN_POINT('Ctrl Pts',(-1.14897523513868,-2.88352007471027,
0.36958303687047));
#26452=CARTESIAN_POINT('Ctrl Pts',(-0.064971125770581,-3.1021061446369,
0.422380613566252));
#26453=CARTESIAN_POINT('Ctrl Pts',(0.864001826933897,-2.81700059999635,
0.475178190262033));
#26454=CARTESIAN_POINT('Ctrl Pts',(1.79297477963837,-2.5318950553558,0.527975766957815));
#26455=CARTESIAN_POINT('Ctrl Pts',(2.56691657567923,-1.74309789614807,0.580773343653596));
#26456=CARTESIAN_POINT('Ctrl Pts',(2.83354070514343,-0.808991748766537,
0.633570920349377));
#26457=CARTESIAN_POINT('Ctrl Pts',(3.10016483460764,0.125114398615,0.686368497045159));
#26458=CARTESIAN_POINT('Ctrl Pts',(2.85947129749519,1.20452953417034,0.73916607374094));
#26459=CARTESIAN_POINT('Ctrl Pts',(2.22094023442363,1.93684572412005,0.791963650436722));
#26460=CARTESIAN_POINT('Ctrl Pts',(1.58240917135208,2.66916191406976,0.844761227132503));
#26461=CARTESIAN_POINT('Ctrl Pts',(0.546040582321433,3.05437915841384,0.897558803828285));
#26462=CARTESIAN_POINT('Ctrl Pts',(-0.415815893186985,2.9172496831673,0.950356380524066));
#26463=CARTESIAN_POINT('Ctrl Pts',(-1.3776723686954,2.78012020792076,1.00315395721985));
#26464=CARTESIAN_POINT('Ctrl Pts',(-2.26501673068159,2.12064401308361,1.05595153391563));
#26465=CARTESIAN_POINT('Ctrl Pts',(-2.67356337698776,1.2391776980577,1.10874911061141));
#26466=CARTESIAN_POINT('Ctrl Pts',(-2.85172980262831,0.854771892525725,
1.13177403471107));
#26467=CARTESIAN_POINT('Ctrl Pts',(-2.93883772557839,0.428147656758027,
1.15479895881073));
#26468=CARTESIAN_POINT('Ctrl Pts',(-2.93753976560994,0.00101398507028504,
1.17782388291039));
#26469=CARTESIAN_POINT('Origin',(0.,0.,0.));
#26470=CARTESIAN_POINT('',(-2.94150578537287,-0.00264448079833085,2.32217611708959));
#26471=CARTESIAN_POINT('',(-2.94148820905054,-0.00265277056903863,2.17782388291039));
#26472=CARTESIAN_POINT('',(-2.942,-3.60291088309151E-16,0.));
#26473=CARTESIAN_POINT('Ctrl Pts',(-2.94150578537287,-0.00264448079833085,
2.32217611708959));
#26474=CARTESIAN_POINT('Ctrl Pts',(-2.93495612048696,0.729051641444702,
2.28259855417621));
#26475=CARTESIAN_POINT('Ctrl Pts',(-2.65840516263949,1.46516741567181,2.24302099126283));
#26476=CARTESIAN_POINT('Ctrl Pts',(-2.16409169020457,2.00002938162346,2.20344342834945));
#26477=CARTESIAN_POINT('Ctrl Pts',(-1.50508163629538,2.71309797609147,2.15067931544623));
#26478=CARTESIAN_POINT('Ctrl Pts',(-0.459025827121477,3.0684629852044,2.097915202543));
#26479=CARTESIAN_POINT('Ctrl Pts',(0.497968791484761,2.90438227824113,2.04515108963977));
#26480=CARTESIAN_POINT('Ctrl Pts',(1.45496341009101,2.74030157127786,1.99238697673655));
#26481=CARTESIAN_POINT('Ctrl Pts',(2.32289683812959,2.05677514823839,1.93962286383332));
#26482=CARTESIAN_POINT('Ctrl Pts',(2.70673338784322,1.16490573313425,1.8868587509301));
#26483=CARTESIAN_POINT('Ctrl Pts',(3.09056993755685,0.273036318030111,1.83409463802687));
#26484=CARTESIAN_POINT('Ctrl Pts',(2.99030960894553,-0.827176089138696,
1.78133052512364));
#26485=CARTESIAN_POINT('Ctrl Pts',(2.4515856938222,-1.63497366892159,1.72856641222042));
#26486=CARTESIAN_POINT('Ctrl Pts',(1.91286177869886,-2.44277124870449,1.67580229931719));
#26487=CARTESIAN_POINT('Ctrl Pts',(0.935674277063515,-2.95815400110147,
1.62303818641397));
#26488=CARTESIAN_POINT('Ctrl Pts',(-0.035215432819809,-2.94655128352351,
1.57027407351074));
#26489=CARTESIAN_POINT('Ctrl Pts',(-1.00610514270313,-2.93494856594555,
1.51750996060752));
#26490=CARTESIAN_POINT('Ctrl Pts',(-1.97069706083443,-2.39636037839263,
1.46474584770429));
#26491=CARTESIAN_POINT('Ctrl Pts',(-2.48996091154496,-1.57591627151309,
1.41198173480107));
#26492=CARTESIAN_POINT('Ctrl Pts',(-2.78456020326321,-1.11044529283744,
1.38204652889724));
#26493=CARTESIAN_POINT('Ctrl Pts',(-2.93581953281605,-0.554251946163811,
1.35211132299342));
#26494=CARTESIAN_POINT('Ctrl Pts',(-2.93759410342513,0.00104371380931417,
1.32217611708959));
#26495=CARTESIAN_POINT('Ctrl Pts',(-2.93753976560994,0.00101398507028504,
1.17782388291039));
#26496=CARTESIAN_POINT('Ctrl Pts',(-2.93586142299925,-0.551296301131853,
1.20759653550651));
#26497=CARTESIAN_POINT('Ctrl Pts',(-2.78636763677815,-1.10445836884475,
1.23736918810263));
#26498=CARTESIAN_POINT('Ctrl Pts',(-2.49479340097823,-1.56829689931507,
1.26714184069876));
#26499=CARTESIAN_POINT('Ctrl Pts',(-1.97772784803637,-2.39084874644727,
1.31993941739454));
#26500=CARTESIAN_POINT('Ctrl Pts',(-1.01384781152648,-2.93249600549699,
1.37273699409032));
#26501=CARTESIAN_POINT('Ctrl Pts',(-0.0423832056000787,-2.94646510892246,
1.4255345707861));
#26502=CARTESIAN_POINT('Ctrl Pts',(0.929081400326319,-2.96043421234793,
1.47833214748188));
#26503=CARTESIAN_POINT('Ctrl Pts',(1.90813057566922,-2.44672516014913,1.53112972417766));
#26504=CARTESIAN_POINT('Ctrl Pts',(2.44864484529323,-1.63940033793356,1.58392730087344));
#26505=CARTESIAN_POINT('Ctrl Pts',(2.98915911491722,-0.832075515717996,
1.63672487756922));
#26506=CARTESIAN_POINT('Ctrl Pts',(3.09113847882232,0.268865076514346,1.68952245426501));
#26507=CARTESIAN_POINT('Ctrl Pts',(2.70810952187376,1.16174019749111,1.74232003096079));
#26508=CARTESIAN_POINT('Ctrl Pts',(2.3250805649252,2.05461531846787,1.79511760765657));
#26509=CARTESIAN_POINT('Ctrl Pts',(1.45704328712297,2.73942496818906,1.84791518435235));
#26510=CARTESIAN_POINT('Ctrl Pts',(0.499541834730426,2.9041250846367,1.90071276104813));
#26511=CARTESIAN_POINT('Ctrl Pts',(-0.457959617662116,3.06882520108433,
1.95351033774391));
#26512=CARTESIAN_POINT('Ctrl Pts',(-1.50492524464497,2.71341578425843,2.00630791443969));
#26513=CARTESIAN_POINT('Ctrl Pts',(-2.16428115211478,1.99984458038746,2.05910549113548));
#26514=CARTESIAN_POINT('Ctrl Pts',(-2.6584810620408,1.4650092650688,2.09867828839378));
#26515=CARTESIAN_POINT('Ctrl Pts',(-2.93492996134342,0.728966169940792,
2.13825108565208));
#26516=CARTESIAN_POINT('Ctrl Pts',(-2.94148820905054,-0.00265277056903863,
2.17782388291039));
#26517=CARTESIAN_POINT('Origin',(0.,0.,0.));
#26518=CARTESIAN_POINT('',(-2.94619134998316,0.00116105206271745,3.3221761170896));
#26519=CARTESIAN_POINT('',(-2.94627397750243,0.0010917140638196,3.17782388291039));
#26520=CARTESIAN_POINT('',(-2.942,-3.60291088309151E-16,0.));
#26521=CARTESIAN_POINT('Ctrl Pts',(-2.94619134998316,0.00116105206271745,
3.3221761170896));
#26522=CARTESIAN_POINT('Ctrl Pts',(-2.94652200322202,0.0667444906727352,
3.31861401116546));
#26523=CARTESIAN_POINT('Ctrl Pts',(-2.94452061107706,0.132307391291658,
3.31505190524133));
#26524=CARTESIAN_POINT('Ctrl Pts',(-2.94012265777212,0.197709134686594,
3.3114897993172));
#26525=CARTESIAN_POINT('Ctrl Pts',(-2.87497745724548,1.16648014993856,3.25872568641397));
#26526=CARTESIAN_POINT('Ctrl Pts',(-2.28399404876592,2.09989107203918,3.20596157351074));
#26527=CARTESIAN_POINT('Ctrl Pts',(-1.43615555362721,2.57310461829436,3.15319746060752));
#26528=CARTESIAN_POINT('Ctrl Pts',(-0.588317058488505,3.04631816454953,
3.10043334770429));
#26529=CARTESIAN_POINT('Ctrl Pts',(0.516376523309347,3.05933433495927,3.04766923480106));
#26530=CARTESIAN_POINT('Ctrl Pts',(1.37512947635203,2.60622889469009,2.99490512189784));
#26531=CARTESIAN_POINT('Ctrl Pts',(2.23388242939471,2.15312345442092,2.94214100899461));
#26532=CARTESIAN_POINT('Ctrl Pts',(2.84669475368223,1.23389640347284,2.88937689609139));
#26533=CARTESIAN_POINT('Ctrl Pts',(2.93464800446939,0.266929283846224,2.83661278318816));
#26534=CARTESIAN_POINT('Ctrl Pts',(3.02260125525656,-0.700037835780391,
2.78384867028493));
#26535=CARTESIAN_POINT('Ctrl Pts',(2.58569543254338,-1.71474502408554,2.73108455738171));
#26536=CARTESIAN_POINT('Ctrl Pts',(1.8227860263141,-2.31535338267893,2.67832044447848));
#26537=CARTESIAN_POINT('Ctrl Pts',(1.05987662008482,-2.91596174127233,2.62555633157526));
#26538=CARTESIAN_POINT('Ctrl Pts',(-0.0290363696605579,-3.10247127015397,
2.57279221867203));
#26539=CARTESIAN_POINT('Ctrl Pts',(-0.948339694866047,-2.78999316350398,
2.52002810576881));
#26540=CARTESIAN_POINT('Ctrl Pts',(-1.86764302007153,-2.47751505685399,
2.46726399286558));
#26541=CARTESIAN_POINT('Ctrl Pts',(-2.61733668073713,-1.66604931467237,
2.41449987996235));
#26542=CARTESIAN_POINT('Ctrl Pts',(-2.85620136174769,-0.724930353670017,
2.36173576705913));
#26543=CARTESIAN_POINT('Ctrl Pts',(-2.91589725889527,-0.489730488784397,
2.34854921706928));
#26544=CARTESIAN_POINT('Ctrl Pts',(-2.94368801886774,-0.24643279880189,
2.33536266707944));
#26545=CARTESIAN_POINT('Ctrl Pts',(-2.94150578537287,-0.00264448079833085,
2.32217611708959));
#26546=CARTESIAN_POINT('Ctrl Pts',(-2.94148820905054,-0.00265277056903863,
2.17782388291039));
#26547=CARTESIAN_POINT('Ctrl Pts',(-2.94367990095588,-0.247151511898062,
2.19104866234787));
#26548=CARTESIAN_POINT('Ctrl Pts',(-2.91572965175503,-0.491156154572101,
2.20427344178534));
#26549=CARTESIAN_POINT('Ctrl Pts',(-2.8556914602692,-0.72699192409469,2.21749822122282));
#26550=CARTESIAN_POINT('Ctrl Pts',(-2.61599967299705,-1.66852423378984,
2.2702957979186));
#26551=CARTESIAN_POINT('Ctrl Pts',(-1.864869910496,-2.47985586226411,2.32309337461438));
#26552=CARTESIAN_POINT('Ctrl Pts',(-0.944572778809107,-2.79128493002216,
2.37589095131016));
#26553=CARTESIAN_POINT('Ctrl Pts',(-0.0242756471222212,-3.1027139977802,
2.42868852800595));
#26554=CARTESIAN_POINT('Ctrl Pts',(1.06518885375051,-2.91424050482202,2.48148610470173));
#26555=CARTESIAN_POINT('Ctrl Pts',(1.82738024207177,-2.31174647809792,2.53428368139751));
#26556=CARTESIAN_POINT('Ctrl Pts',(2.58957163039303,-1.70925245137381,2.58708125809329));
#26557=CARTESIAN_POINT('Ctrl Pts',(3.02448990616283,-0.692737890883784,
2.63987883478907));
#26558=CARTESIAN_POINT('Ctrl Pts',(2.93395403704711,0.274597720394451,2.69267641148485));
#26559=CARTESIAN_POINT('Ctrl Pts',(2.8434181679314,1.24193333167269,2.74547398818063));
#26560=CARTESIAN_POINT('Ctrl Pts',(2.22742815393017,2.16008999373912,2.79827156487642));
#26561=CARTESIAN_POINT('Ctrl Pts',(1.36667466982157,2.61068771331245,2.8510691415722));
#26562=CARTESIAN_POINT('Ctrl Pts',(0.505921185712974,3.06128543288579,2.90386671826798));
#26563=CARTESIAN_POINT('Ctrl Pts',(-0.599595768502999,3.04432420996601,
2.95666429496376));
#26564=CARTESIAN_POINT('Ctrl Pts',(-1.44612088828002,2.56753276921717,3.00946187165954));
#26565=CARTESIAN_POINT('Ctrl Pts',(-2.29264600805703,2.09074132846833,3.06225944835532));
#26566=CARTESIAN_POINT('Ctrl Pts',(-2.8801792933951,1.15411966989042,3.1150570250511));
#26567=CARTESIAN_POINT('Ctrl Pts',(-2.9409970926588,0.184461960144107,3.16785460174689));
#26568=CARTESIAN_POINT('Ctrl Pts',(-2.94482498135212,0.123431442294656,
3.17117769546805));
#26569=CARTESIAN_POINT('Ctrl Pts',(-2.9465662984666,0.0622700528698149,
3.17450078918922));
#26570=CARTESIAN_POINT('Ctrl Pts',(-2.94627397750243,0.0010917140638196,
3.17782388291039));
#26571=CARTESIAN_POINT('Origin',(0.,0.,0.));
#26572=CARTESIAN_POINT('',(-2.93825501966817,0.00168812480491387,4.3221761170896));
#26573=CARTESIAN_POINT('',(-2.93839638220268,0.00179748935179793,4.17782388291039));
#26574=CARTESIAN_POINT('',(-2.942,-3.60291088309151E-16,0.));
#26575=CARTESIAN_POINT('Ctrl Pts',(-2.93825501966817,0.00168812480491387,
4.3221761170896));
#26576=CARTESIAN_POINT('Ctrl Pts',(-2.94023496409179,0.378238072324008,
4.30186535525148));
#26577=CARTESIAN_POINT('Ctrl Pts',(-2.87305142275175,0.754108328434651,
4.28155459341337));
#26578=CARTESIAN_POINT('Ctrl Pts',(-2.73342934159449,1.1008061494448,4.26124383157526));
#26579=CARTESIAN_POINT('Ctrl Pts',(-2.3707134911166,2.00147167429752,4.20847971867203));
#26580=CARTESIAN_POINT('Ctrl Pts',(-1.51912634074217,2.70525904140838,4.15571560576881));
#26581=CARTESIAN_POINT('Ctrl Pts',(-0.566263490800549,2.89184297694709,
4.10295149286558));
#26582=CARTESIAN_POINT('Ctrl Pts',(0.38659935914108,3.07842691248581,4.05018737996236));
#26583=CARTESIAN_POINT('Ctrl Pts',(1.44073790864989,2.74780741645236,3.99742326705913));
#26584=CARTESIAN_POINT('Ctrl Pts',(2.1163663088001,2.05046428665802,3.9446591541559));
#26585=CARTESIAN_POINT('Ctrl Pts',(2.79199470895031,1.35312115686368,3.89189504125268));
#26586=CARTESIAN_POINT('Ctrl Pts',(3.08911295974191,0.289054393308455,3.83913092834945));
#26587=CARTESIAN_POINT('Ctrl Pts',(2.87248918644939,-0.657431378827086,
3.78636681544623));
#26588=CARTESIAN_POINT('Ctrl Pts',(2.65586541315687,-1.60391715096264,3.733602702543));
#26589=CARTESIAN_POINT('Ctrl Pts',(1.9254996157802,-2.4328219316785,3.68083858963977));
#26590=CARTESIAN_POINT('Ctrl Pts',(1.01381410678357,-2.76687388619937,3.62807447673655));
#26591=CARTESIAN_POINT('Ctrl Pts',(0.102128597786946,-3.10092584072023,
3.57531036383332));
#26592=CARTESIAN_POINT('Ctrl Pts',(-0.990876622829635,-2.94012496904611,
3.5225462509301));
#26593=CARTESIAN_POINT('Ctrl Pts',(-1.76772573685106,-2.35765897900741,
3.46978213802687));
#26594=CARTESIAN_POINT('Ctrl Pts',(-2.4921297574377,-1.81451527526447,3.42058013104778));
#26595=CARTESIAN_POINT('Ctrl Pts',(-2.94162416323671,-0.904717906319905,
3.37137812406869));
#26596=CARTESIAN_POINT('Ctrl Pts',(-2.94619134998316,0.00116105206271745,
3.3221761170896));
#26597=CARTESIAN_POINT('Ctrl Pts',(-2.94627397750243,0.0010917140638196,
3.17782388291039));
#26598=CARTESIAN_POINT('Ctrl Pts',(-2.94192187979514,-0.909736247962167,
3.227298365885));
#26599=CARTESIAN_POINT('Ctrl Pts',(-2.48680392404959,-1.82432112348186,
3.27677284885962));
#26600=CARTESIAN_POINT('Ctrl Pts',(-1.75560149895312,-2.36671786778377,
3.32624733183423));
#26601=CARTESIAN_POINT('Ctrl Pts',(-0.97528579279443,-2.9455462250506,3.37904490853001));
#26602=CARTESIAN_POINT('Ctrl Pts',(0.119447932712268,-3.10050917866955,
3.43184248522579));
#26603=CARTESIAN_POINT('Ctrl Pts',(1.02975799022302,-2.76099413129472,3.48464006192158));
#26604=CARTESIAN_POINT('Ctrl Pts',(1.94006804773377,-2.42147908391989,3.53743763861736));
#26605=CARTESIAN_POINT('Ctrl Pts',(2.66595443724857,-1.58748603555126,3.59023521531314));
#26606=CARTESIAN_POINT('Ctrl Pts',(2.87664960568935,-0.639043935488772,
3.64303279200892));
#26607=CARTESIAN_POINT('Ctrl Pts',(3.08734477413012,0.309398164573712,3.6958303687047));
#26608=CARTESIAN_POINT('Ctrl Pts',(2.78284872149689,1.37228931633006,3.74862794540048));
#26609=CARTESIAN_POINT('Ctrl Pts',(2.10191238159562,2.06529766444029,3.80142552209626));
#26610=CARTESIAN_POINT('Ctrl Pts',(1.42097604169435,2.75830601255052,3.85422309879205));
#26611=CARTESIAN_POINT('Ctrl Pts',(0.363599414525042,3.08143155701465,3.90702067548783));
#26612=CARTESIAN_POINT('Ctrl Pts',(-0.588398467996306,2.88743438864685,
3.95981825218361));
#26613=CARTESIAN_POINT('Ctrl Pts',(-1.54039635051765,2.69343722027906,4.01261582887939));
#26614=CARTESIAN_POINT('Ctrl Pts',(-2.38701548839103,1.98231733907935,4.06541340557517));
#26615=CARTESIAN_POINT('Ctrl Pts',(-2.7424735561947,1.07811358323904,4.11821098227095));
#26616=CARTESIAN_POINT('Ctrl Pts',(-2.87625423202358,0.73780624321788,4.13808194915077));
#26617=CARTESIAN_POINT('Ctrl Pts',(-2.94046299306174,0.370148985435419,
4.15795291603058));
#26618=CARTESIAN_POINT('Ctrl Pts',(-2.93839638220268,0.00179748935179793,
4.17782388291039));
#26619=CARTESIAN_POINT('Origin',(0.,0.,0.));
#26620=CARTESIAN_POINT('',(-2.940183414122,-0.00248894513365655,5.32217611708959));
#26621=CARTESIAN_POINT('',(-2.93985340888279,-0.00241994382505922,5.17782388291038));
#26622=CARTESIAN_POINT('',(-2.942,-3.60291088309151E-16,0.));
#26623=CARTESIAN_POINT('Ctrl Pts',(-2.940183414122,-0.00248894513365655,
5.32217611708959));
#26624=CARTESIAN_POINT('Ctrl Pts',(-2.93461614813994,0.683436241442127,
5.28511669933751));
#26625=CARTESIAN_POINT('Ctrl Pts',(-2.69512958010689,1.37286568437424,5.24805728158542));
#26626=CARTESIAN_POINT('Ctrl Pts',(-2.2565518807566,1.89509465558241,5.21099786383333));
#26627=CARTESIAN_POINT('Ctrl Pts',(-1.6321178057218,2.63862895993905,5.1582337509301));
#26628=CARTESIAN_POINT('Ctrl Pts',(-0.604101521911408,3.04322734464819,
5.10546963802687));
#26629=CARTESIAN_POINT('Ctrl Pts',(0.35960053931388,2.92473889369513,5.05270552512364));
#26630=CARTESIAN_POINT('Ctrl Pts',(1.32330260053916,2.80625044274206,4.99994141222042));
#26631=CARTESIAN_POINT('Ctrl Pts',(2.22269043917934,2.16467515612679,4.94717729931719));
#26632=CARTESIAN_POINT('Ctrl Pts',(2.64841221253011,1.29202279263227,4.89441318641397));
#26633=CARTESIAN_POINT('Ctrl Pts',(3.07413398588089,0.419370429137726,4.84164907351074));
#26634=CARTESIAN_POINT('Ctrl Pts',(3.02618969394223,-0.684359011236085,
4.78888496060752));
#26635=CARTESIAN_POINT('Ctrl Pts',(2.52640093959537,-1.51680863544845,4.73612084770429));
#26636=CARTESIAN_POINT('Ctrl Pts',(2.02661218524851,-2.34925825966081,4.68335673480107));
#26637=CARTESIAN_POINT('Ctrl Pts',(1.07497896849345,-2.91042806771174,4.63059262189784));
#26638=CARTESIAN_POINT('Ctrl Pts',(0.104632352620345,-2.94490444920961,
4.57782850899461));
#26639=CARTESIAN_POINT('Ctrl Pts',(-0.86571426325276,-2.97938083070748,
4.52506439609139));
#26640=CARTESIAN_POINT('Ctrl Pts',(-1.8547742782439,-2.4871637856523,4.47230028318816));
#26641=CARTESIAN_POINT('Ctrl Pts',(-2.41238201044881,-1.69228342182741,
4.41953617028494));
#26642=CARTESIAN_POINT('Ctrl Pts',(-2.75534692531544,-1.20338045193787,
4.38708281921983));
#26643=CARTESIAN_POINT('Ctrl Pts',(-2.93509138494185,-0.599978505811401,
4.35462946815471));
#26644=CARTESIAN_POINT('Ctrl Pts',(-2.93825501966817,0.00168812480491387,
4.3221761170896));
#26645=CARTESIAN_POINT('Ctrl Pts',(-2.93839638220268,0.00179748935179793,
4.17782388291039));
#26646=CARTESIAN_POINT('Ctrl Pts',(-2.93497196456819,-0.608568682562856,
4.21075049272636));
#26647=CARTESIAN_POINT('Ctrl Pts',(-2.74957402147642,-1.22084103753697,
4.24367710254233));
#26648=CARTESIAN_POINT('Ctrl Pts',(-2.39720087876282,-1.71374386983141,
4.2766037123583));
#26649=CARTESIAN_POINT('Ctrl Pts',(-1.83217313579332,-2.50410993658064,
4.32940128905408));
#26650=CARTESIAN_POINT('Ctrl Pts',(-0.837820652120374,-2.98755443959817,
4.38219886574986));
#26651=CARTESIAN_POINT('Ctrl Pts',(0.132756003210123,-2.9437842904309,4.43499644244564));
#26652=CARTESIAN_POINT('Ctrl Pts',(1.10333265854061,-2.90001414126364,4.48779401914142));
#26653=CARTESIAN_POINT('Ctrl Pts',(2.05013348552865,-2.32902933991158,4.5405915958372));
#26654=CARTESIAN_POINT('Ctrl Pts',(2.5417259684161,-1.4910128122426,4.59338917253299));
#26655=CARTESIAN_POINT('Ctrl Pts',(3.03331845130357,-0.652996284573612,
4.64618674922877));
#26656=CARTESIAN_POINT('Ctrl Pts',(3.06970259009044,0.452051969412309,4.69898432592455));
#26657=CARTESIAN_POINT('Ctrl Pts',(2.63429907890363,1.32059019671555,4.75178190262033));
#26658=CARTESIAN_POINT('Ctrl Pts',(2.19889556771682,2.18912842401878,4.80457947931611));
#26659=CARTESIAN_POINT('Ctrl Pts',(1.29170440655633,2.82115662463934,4.85737705601189));
#26660=CARTESIAN_POINT('Ctrl Pts',(0.326109016449051,2.92867598314074,4.91017463270768));
#26661=CARTESIAN_POINT('Ctrl Pts',(-0.639486373658232,3.03619534164214,
4.96297220940346));
#26662=CARTESIAN_POINT('Ctrl Pts',(-1.66348599271231,2.61920585802438,5.01576978609924));
#26663=CARTESIAN_POINT('Ctrl Pts',(-2.2792798429615,1.86771879635947,5.06856736279502));
#26664=CARTESIAN_POINT('Ctrl Pts',(-2.70404361305101,1.34935623499724,5.10498620283347));
#26665=CARTESIAN_POINT('Ctrl Pts',(-2.93458316728716,0.671839798883881,
5.14140504287193));
#26666=CARTESIAN_POINT('Ctrl Pts',(-2.93985340888279,-0.00241994382505922,
5.17782388291038));
#26667=CARTESIAN_POINT('Origin',(0.,0.,0.));
#26668=CARTESIAN_POINT('',(-2.94670914091441,0.000353147988772619,6.3221761170896));
#26669=CARTESIAN_POINT('',(-2.94677477477595,5.75751945360796E-5,6.17782388291039));
#26670=CARTESIAN_POINT('',(-2.942,-3.60291088309151E-16,0.));
#26671=CARTESIAN_POINT('Ctrl Pts',(-2.94670914091441,0.000353147988772619,
6.3221761170896));
#26672=CARTESIAN_POINT('Ctrl Pts',(-2.94674188304789,0.0195649300909904,
6.32113215632675));
#26673=CARTESIAN_POINT('Ctrl Pts',(-2.94657014404334,0.0387761113611483,
6.32008819556391));
#26674=CARTESIAN_POINT('Ctrl Pts',(-2.94619213372924,0.0579832330598756,
6.31904423480106));
#26675=CARTESIAN_POINT('Ctrl Pts',(-2.92708664662515,1.02875414124661,6.26628012189784));
#26676=CARTESIAN_POINT('Ctrl Pts',(-2.38105743179868,1.98915480203517,6.21351600899462));
#26677=CARTESIAN_POINT('Ctrl Pts',(-1.55662693491459,2.50206369416578,6.16075189609139));
#26678=CARTESIAN_POINT('Ctrl Pts',(-0.732196438030497,3.01497258629639,
6.10798778318816));
#26679=CARTESIAN_POINT('Ctrl Pts',(0.370635340911205,3.08038970976906,6.05522367028493));
#26680=CARTESIAN_POINT('Ctrl Pts',(1.24992007493953,2.6685407904747,6.00245955738171));
#26681=CARTESIAN_POINT('Ctrl Pts',(2.12920480896786,2.25669187118035,5.94969544447848));
#26682=CARTESIAN_POINT('Ctrl Pts',(2.78494249808281,1.36757690911897,5.89693133157526));
#26683=CARTESIAN_POINT('Ctrl Pts',(2.91867743737271,0.405872098986324,5.84416721867204));
#26684=CARTESIAN_POINT('Ctrl Pts',(3.0524123766626,-0.555832711146327,5.79140310576881));
#26685=CARTESIAN_POINT('Ctrl Pts',(2.66414456612744,-1.59012736935025,5.73863899286558));
#26686=CARTESIAN_POINT('Ctrl Pts',(1.93059214323493,-2.22625787379709,5.68587487996235));
#26687=CARTESIAN_POINT('Ctrl Pts',(1.19703972034241,-2.86238837824392,5.63311076705913));
#26688=CARTESIAN_POINT('Ctrl Pts',(0.118202685092545,-3.10035472893366,
5.58034665415591));
#26689=CARTESIAN_POINT('Ctrl Pts',(-0.81489172222448,-2.8318477404717,5.52758254125268));
#26690=CARTESIAN_POINT('Ctrl Pts',(-1.7479861295415,-2.56334075200975,5.47481842834945));
#26691=CARTESIAN_POINT('Ctrl Pts',(-2.53533790892568,-1.78836042439612,
5.42205431544622));
#26692=CARTESIAN_POINT('Ctrl Pts',(-2.81858786548815,-0.859635148587238,
5.369290202543));
#26693=CARTESIAN_POINT('Ctrl Pts',(-2.90289429981681,-0.58320962879346,
5.35358550739186));
#26694=CARTESIAN_POINT('Ctrl Pts',(-2.94254265828655,-0.293163936945955,
5.33788081224073));
#26695=CARTESIAN_POINT('Ctrl Pts',(-2.940183414122,-0.00248894513365655,
5.32217611708959));
#26696=CARTESIAN_POINT('Ctrl Pts',(-2.93985340888279,-0.00241994382505923,
5.17782388291039));
#26697=CARTESIAN_POINT('Ctrl Pts',(-2.94222360790956,-0.305656476147461,
5.19420261956771));
#26698=CARTESIAN_POINT('Ctrl Pts',(-2.89903098481243,-0.608234311816698,
5.21058135622504));
#26699=CARTESIAN_POINT('Ctrl Pts',(-2.80745159681895,-0.895380163016774,
5.22696009288236));
#26700=CARTESIAN_POINT('Ctrl Pts',(-2.51224141898293,-1.82100742101599,
5.27975766957815));
#26701=CARTESIAN_POINT('Ctrl Pts',(-1.71423298186661,-2.58627729730233,
5.33255524627393));
#26702=CARTESIAN_POINT('Ctrl Pts',(-0.777057978406682,-2.8424762097523,
5.38535282296971));
#26703=CARTESIAN_POINT('Ctrl Pts',(0.160117025053262,-3.09867512220227,
5.43815039966549));
#26704=CARTESIAN_POINT('Ctrl Pts',(1.23645859485682,-2.84580307081584,5.49094797636127));
#26705=CARTESIAN_POINT('Ctrl Pts',(1.96150586742938,-2.19908727358619,5.54374555305705));
#26706=CARTESIAN_POINT('Ctrl Pts',(2.68655314000193,-1.55237147635655,5.59654312975283));
#26707=CARTESIAN_POINT('Ctrl Pts',(3.06030611534348,-0.511811933283709,
5.64934070644862));
#26708=CARTESIAN_POINT('Ctrl Pts',(2.91245528187179,0.448435431144968,5.7021382831444));
#26709=CARTESIAN_POINT('Ctrl Pts',(2.76460444840011,1.40868279557365,5.75493585984018));
#26710=CARTESIAN_POINT('Ctrl Pts',(2.09514980611517,2.28861798135817,5.80773343653596));
#26711=CARTESIAN_POINT('Ctrl Pts',(1.2091444266347,2.68727740666057,5.86053101323174));
#26712=CARTESIAN_POINT('Ctrl Pts',(0.323139047154223,3.08593683196296,5.91332858992752));
#26713=CARTESIAN_POINT('Ctrl Pts',(-0.779417069521796,3.00332049678325,
5.9661261666233));
#26714=CARTESIAN_POINT('Ctrl Pts',(-1.59611777250727,2.47707451666191,6.01892374331908));
#26715=CARTESIAN_POINT('Ctrl Pts',(-2.41281847549274,1.95082853654058,6.07172132001487));
#26716=CARTESIAN_POINT('Ctrl Pts',(-2.94366376478766,0.980952911477632,
6.12451889671065));
#26717=CARTESIAN_POINT('Ctrl Pts',(-2.94676124645694,0.00939474262821921,
6.17731647340643));
#26718=CARTESIAN_POINT('Ctrl Pts',(-2.94677116920804,0.00628236589065139,
6.17748560990775));
#26719=CARTESIAN_POINT('Ctrl Pts',(-2.94677567602789,0.0031699718862354,
6.17765474640907));
#26720=CARTESIAN_POINT('Ctrl Pts',(-2.94677477477595,5.75751945359972E-5,
6.17782388291039));
#26721=CARTESIAN_POINT('Origin',(0.,0.,0.));
#26722=CARTESIAN_POINT('',(-2.93921061841706,0.00219993862087403,7.3221761170896));
#26723=CARTESIAN_POINT('',(-2.9396928876012,0.00237510757666561,7.17782388291039));
#26724=CARTESIAN_POINT('',(-2.942,-3.60291088309151E-16,0.));
#26725=CARTESIAN_POINT('Ctrl Pts',(-2.93921061841706,0.00219993862087403,
7.3221761170896));
#26726=CARTESIAN_POINT('Ctrl Pts',(-2.94151862483926,0.331795310107375,
7.30438350041277));
#26727=CARTESIAN_POINT('Ctrl Pts',(-2.89034506178059,0.660694979142846,
7.28659088373595));
#26728=CARTESIAN_POINT('Ctrl Pts',(-2.78258184963522,0.969870297640249,
7.26879826705912));
#26729=CARTESIAN_POINT('Ctrl Pts',(-2.46300938900557,1.8867315838915,7.2160341541559));
#26730=CARTESIAN_POINT('Ctrl Pts',(-1.64577474805962,2.63013246788686,7.16327004125268));
#26731=CARTESIAN_POINT('Ctrl Pts',(-0.702838155545203,2.86171778330323,
7.11050592834945));
#26732=CARTESIAN_POINT('Ctrl Pts',(0.24009843696921,3.0933030987196,7.05774181544623));
#26733=CARTESIAN_POINT('Ctrl Pts',(1.30873698105206,2.81307284555698,7.004977702543));
#26734=CARTESIAN_POINT('Ctrl Pts',(2.01669202827731,2.14857241145066,6.95221358963978));
#26735=CARTESIAN_POINT('Ctrl Pts',(2.72464707550255,1.48407197734434,6.89944947673655));
#26736=CARTESIAN_POINT('Ctrl Pts',(3.07191862587017,0.435301362294284,6.84668536383332));
#26737=CARTESIAN_POINT('Ctrl Pts',(2.90044778314584,-0.520396773057355,
6.7939212509301));
#26738=CARTESIAN_POINT('Ctrl Pts',(2.72897694042151,-1.476094908409,6.74115713802687));
#26739=CARTESIAN_POINT('Ctrl Pts',(2.03876370460524,-2.33872056406225,6.68839302512365));
#26740=CARTESIAN_POINT('Ctrl Pts',(1.14395515196615,-2.7156540196524,6.63562891222042));
#26741=CARTESIAN_POINT('Ctrl Pts',(0.249146599327066,-3.09258747524255,
6.58286479931719));
#26742=CARTESIAN_POINT('Ctrl Pts',(-0.850257270134833,-2.98382873076961,
6.53010068641397));
#26743=CARTESIAN_POINT('Ctrl Pts',(-1.65386832517493,-2.43887878074069,
6.47733657351074));
#26744=CARTESIAN_POINT('Ctrl Pts',(-2.44157958840789,-1.90471090083939,
6.42561642137036));
#26745=CARTESIAN_POINT('Ctrl Pts',(-2.94508702235829,-0.95144152531619,
6.37389626922998));
#26746=CARTESIAN_POINT('Ctrl Pts',(-2.94670914091441,0.000353147988772619,
6.3221761170896));
#26747=CARTESIAN_POINT('Ctrl Pts',(-2.94677477477595,5.75751945360796E-5,
6.17782388291039));
#26748=CARTESIAN_POINT('Ctrl Pts',(-2.94649434161591,-0.96839442583636,
6.23045232310485));
#26749=CARTESIAN_POINT('Ctrl Pts',(-2.42260291217609,-1.93710661038694,
6.28308076329931));
#26750=CARTESIAN_POINT('Ctrl Pts',(-1.61187977882684,-2.46684691122469,
6.33570920349377));
#26751=CARTESIAN_POINT('Ctrl Pts',(-0.798551155483845,-2.99828968359228,
6.38850678018955));
#26752=CARTESIAN_POINT('Ctrl Pts',(0.303455765245771,-3.08793451569159,
6.44130435688534));
#26753=CARTESIAN_POINT('Ctrl Pts',(1.19198508678719,-2.69493258870913,6.49410193358112));
#26754=CARTESIAN_POINT('Ctrl Pts',(2.0805144083286,-2.30193066172667,6.5468995102769));
#26755=CARTESIAN_POINT('Ctrl Pts',(2.75556613068181,-1.42628197566246,6.59969708697268));
#26756=CARTESIAN_POINT('Ctrl Pts',(2.90953673839141,-0.466996865899832,
6.65249466366846));
#26757=CARTESIAN_POINT('Ctrl Pts',(3.063507346101,0.492288243862799,6.70529224036424));
#26758=CARTESIAN_POINT('Ctrl Pts',(2.69639683916696,1.53520977732385,6.75808981706003));
#26759=CARTESIAN_POINT('Ctrl Pts',(1.97548792905307,2.18653551239746,6.81088739375581));
#26760=CARTESIAN_POINT('Ctrl Pts',(1.25457901893917,2.83786124747105,6.86368497045159));
#26761=CARTESIAN_POINT('Ctrl Pts',(0.179871705645437,3.09759118415722,6.91648254714737));
#26762=CARTESIAN_POINT('Ctrl Pts',(-0.758917835447689,2.84737314447,6.96928012384315));
#26763=CARTESIAN_POINT('Ctrl Pts',(-1.69770737654082,2.59715510478277,7.02207770053893));
#26764=CARTESIAN_POINT('Ctrl Pts',(-2.50057914543333,1.83698908872215,7.07487527723471));
#26765=CARTESIAN_POINT('Ctrl Pts',(-2.80168535536551,0.913262982026531,
7.1276728539305));
#26766=CARTESIAN_POINT('Ctrl Pts',(-2.89702297756577,0.620788606966313,
7.14438986359046));
#26767=CARTESIAN_POINT('Ctrl Pts',(-2.94205804349871,0.3119171506092,7.16110687325043));
#26768=CARTESIAN_POINT('Ctrl Pts',(-2.9396928876012,0.00237510757666561,
7.17782388291039));
#26769=CARTESIAN_POINT('Origin',(0.,0.,0.));
#26770=CARTESIAN_POINT('',(-2.93902884880934,-0.00212417613307953,8.3221761170896));
#26771=CARTESIAN_POINT('',(-2.93851596067447,-0.00187194491636513,8.17782388291039));
#26772=CARTESIAN_POINT('',(-2.942,-3.60291088309151E-16,0.));
#26773=CARTESIAN_POINT('Ctrl Pts',(-2.93902884880934,-0.00212417613307953,
8.3221761170896));
#26774=CARTESIAN_POINT('Ctrl Pts',(-2.93472032584333,0.63782764634564,8.2876348444988));
#26775=CARTESIAN_POINT('Ctrl Pts',(-2.72915033143689,1.28029955423599,8.25309357190799));
#26776=CARTESIAN_POINT('Ctrl Pts',(-2.34392897127172,1.78589112820386,8.21855229931719));
#26777=CARTESIAN_POINT('Ctrl Pts',(-1.75547748075246,2.55821620168318,8.16578818641397));
#26778=CARTESIAN_POINT('Ctrl Pts',(-0.747816469944497,3.01113630499568,
8.11302407351074));
#26779=CARTESIAN_POINT('Ctrl Pts',(0.220422229727873,2.93850713540157,8.06025996060752));
#26780=CARTESIAN_POINT('Ctrl Pts',(1.18866092940026,2.86587796580745,8.00749584770429));
#26781=CARTESIAN_POINT('Ctrl Pts',(2.11747731793707,2.26769952330669,7.95473173480106));
#26782=CARTESIAN_POINT('Ctrl Pts',(2.58412529643943,1.41622971175793,7.90196762189784));
#26783=CARTESIAN_POINT('Ctrl Pts',(3.05077327494178,0.564759900209195,7.84920350899461));
#26784=CARTESIAN_POINT('Ctrl Pts',(3.05525284340971,-0.540001280387511,
7.79643939609139));
#26785=CARTESIAN_POINT('Ctrl Pts',(2.59552514882778,-1.3952273456203,7.74367528318817));
#26786=CARTESIAN_POINT('Ctrl Pts',(2.13579745424584,-2.25045341085309,7.69091117028494));
#26787=CARTESIAN_POINT('Ctrl Pts',(1.21186249661401,-2.85614436072195,7.63814705738171));
#26788=CARTESIAN_POINT('Ctrl Pts',(0.244244616152473,-2.93662301149546,
7.58538294447848));
#26789=CARTESIAN_POINT('Ctrl Pts',(-0.723373264309057,-3.01710166226897,
7.53261883157526));
#26790=CARTESIAN_POINT('Ctrl Pts',(-1.7346740676003,-2.57236801394714,7.47985471867203));
#26791=CARTESIAN_POINT('Ctrl Pts',(-2.32936932908925,-1.80484034553266,
7.42709060576881));
#26792=CARTESIAN_POINT('Ctrl Pts',(-2.72352706147006,-1.29613112097227,
7.3921191095424));
#26793=CARTESIAN_POINT('Ctrl Pts',(-2.93467421776558,-0.645621767401394,
7.357147613316));
#26794=CARTESIAN_POINT('Ctrl Pts',(-2.93921061841706,0.00219993862087403,
7.3221761170896));
#26795=CARTESIAN_POINT('Ctrl Pts',(-2.9396928876012,0.00237510757666561,
7.17782388291039));
#26796=CARTESIAN_POINT('Ctrl Pts',(-2.93458813695223,-0.665714022071069,
7.21390444994621));
#26797=CARTESIAN_POINT('Ctrl Pts',(-2.70867788182517,-1.33692696049954,
7.24998501698203));
#26798=CARTESIAN_POINT('Ctrl Pts',(-2.29114255557572,-1.85314756423755,
7.28606558401784));
#26799=CARTESIAN_POINT('Ctrl Pts',(-1.68015289488189,-2.60854580647539,
7.33886316071362));
#26800=CARTESIAN_POINT('Ctrl Pts',(-0.658832922522417,-3.03205609362045,
7.3916607374094));
#26801=CARTESIAN_POINT('Ctrl Pts',(0.307428409071859,-2.9306958010181,7.44445831410518));
#26802=CARTESIAN_POINT('Ctrl Pts',(1.27368974066613,-2.82933550841574,7.49725589080096));
#26803=CARTESIAN_POINT('Ctrl Pts',(2.18489243149519,-2.20310463606597,7.55005346749675));
#26804=CARTESIAN_POINT('Ctrl Pts',(2.62582511077046,-1.33736030764222,7.60285104419253));
#26805=CARTESIAN_POINT('Ctrl Pts',(3.06675779004572,-0.471615979218467,
7.65564862088831));
#26806=CARTESIAN_POINT('Ctrl Pts',(3.03742045776721,0.633641805279265,7.70844619758409));
#26807=CARTESIAN_POINT('Ctrl Pts',(2.5511813733499,1.47477581519432,7.76124377427987));
#26808=CARTESIAN_POINT('Ctrl Pts',(2.0649422889326,2.31590982510937,7.81404135097565));
#26809=CARTESIAN_POINT('Ctrl Pts',(1.12180145237649,2.89292006044175,7.86683892767144));
#26810=CARTESIAN_POINT('Ctrl Pts',(0.151523616940655,2.94287796184599,7.91963650436722));
#26811=CARTESIAN_POINT('Ctrl Pts',(-0.818754218495187,2.99283586325022,
7.972434081063));
#26812=CARTESIAN_POINT('Ctrl Pts',(-1.81616905281075,2.51574143072631,8.02523165775878));
#26813=CARTESIAN_POINT('Ctrl Pts',(-2.38622488333927,1.72899419054607,8.07802923445456));
#26814=CARTESIAN_POINT('Ctrl Pts',(-2.74538607196463,1.2333075247876,8.11129411727317));
#26815=CARTESIAN_POINT('Ctrl Pts',(-2.93490389706639,0.614701853345732,
8.14455900009178));
#26816=CARTESIAN_POINT('Ctrl Pts',(-2.93851596067447,-0.00187194491636513,
8.17782388291039));
#26817=CARTESIAN_POINT('Origin',(0.,0.,0.));
#26818=CARTESIAN_POINT('',(-2.94665746643035,-0.000496894171833351,9.3221761170896));
#26819=CARTESIAN_POINT('',(-2.94636616095733,-0.000987191619394096,9.17782388291039));
#26820=CARTESIAN_POINT('',(-2.942,-3.60291088309151E-16,0.));
#26821=CARTESIAN_POINT('Ctrl Pts',(-2.94665746643035,-0.000496894171833351,
9.3221761170896));
#26822=CARTESIAN_POINT('Ctrl Pts',(-2.94443817053572,0.943424973374663,
9.27088618858482));
#26823=CARTESIAN_POINT('Ctrl Pts',(-2.45042926639946,1.88934479557273,9.21959626008003));
#26824=CARTESIAN_POINT('Ctrl Pts',(-1.67359187304369,2.42538664683515,9.16830633157526));
#26825=CARTESIAN_POINT('Ctrl Pts',(-0.874426478873733,2.9768355099044,9.11554221867203));
#26826=CARTESIAN_POINT('Ctrl Pts',(0.224059267942015,3.09450622303989,9.06277810576881));
#26827=CARTESIAN_POINT('Ctrl Pts',(1.12189511505486,2.72484155410552,9.01001399286558));
#26828=CARTESIAN_POINT('Ctrl Pts',(2.01973096216771,2.35517688517114,8.95724987996236));
#26829=CARTESIAN_POINT('Ctrl Pts',(2.71691690957765,1.49817683416691,8.90448576705913));
#26830=CARTESIAN_POINT('Ctrl Pts',(2.89613228646949,0.54390065584916,8.8517216541559));
#26831=CARTESIAN_POINT('Ctrl Pts',(3.07534766336132,-0.410375522468571,
8.79895754125268));
#26832=CARTESIAN_POINT('Ctrl Pts',(2.73659246973507,-1.46192782809981,8.74619342834945));
#26833=CARTESIAN_POINT('Ctrl Pts',(2.03404942496847,-2.13214752795147,8.69342931544623));
#26834=CARTESIAN_POINT('Ctrl Pts',(1.33150638020187,-2.80236722780314,8.640665202543));
#26835=CARTESIAN_POINT('Ctrl Pts',(0.265175484294899,-3.09125432187523,
8.58790108963977));
#26836=CARTESIAN_POINT('Ctrl Pts',(-0.679608128765257,-2.86732330501468,
8.53513697673655));
#26837=CARTESIAN_POINT('Ctrl Pts',(-1.62439174182541,-2.64339228815413,
8.48237286383332));
#26838=CARTESIAN_POINT('Ctrl Pts',(-2.44762807203876,-1.90664316036094,
8.4296087509301));
#26839=CARTESIAN_POINT('Ctrl Pts',(-2.77462525203015,-0.992403574641266,
8.37684463802687));
#26840=CARTESIAN_POINT('Ctrl Pts',(-2.88755840044724,-0.676657870578698,
8.35862179771445));
#26841=CARTESIAN_POINT('Ctrl Pts',(-2.94130188393814,-0.339741727368865,
8.34039895740202));
#26842=CARTESIAN_POINT('Ctrl Pts',(-2.93902884880934,-0.00212417613307953,
8.3221761170896));
#26843=CARTESIAN_POINT('Ctrl Pts',(-2.93851596067447,-0.00187194491636513,
8.17782388291039));
#26844=CARTESIAN_POINT('Ctrl Pts',(-2.94063691607077,-0.363915825239363,
8.19735657678756));
#26845=CARTESIAN_POINT('Ctrl Pts',(-2.87865977372572,-0.725259139831482,
8.21688927066473));
#26846=CARTESIAN_POINT('Ctrl Pts',(-2.74929213038533,-1.06060496256188,
8.23642196454191));
#26847=CARTESIAN_POINT('Ctrl Pts',(-2.39960672016141,-1.96705682765307,
8.28921954123769));
#26848=CARTESIAN_POINT('Ctrl Pts',(-1.55753907297209,-2.6835605099989,8.34201711793347));
#26849=CARTESIAN_POINT('Ctrl Pts',(-0.606797518045518,-2.88362391391516,
8.39481469462925));
#26850=CARTESIAN_POINT('Ctrl Pts',(0.343944036881066,-3.08368731783141,
8.44761227132503));
#26851=CARTESIAN_POINT('Ctrl Pts',(1.40335949954491,-2.7673104433181,8.50040984802081));
#26852=CARTESIAN_POINT('Ctrl Pts',(2.0887007932398,-2.07865800485049,8.55320742471659));
#26853=CARTESIAN_POINT('Ctrl Pts',(2.77404208693468,-1.39000556638288,8.60600500141238));
#26854=CARTESIAN_POINT('Ctrl Pts',(3.08530921166061,-0.329077563960986,
8.65880257810816));
#26855=CARTESIAN_POINT('Ctrl Pts',(2.88066583304364,0.62068870067415,8.71160015480394));
#26856=CARTESIAN_POINT('Ctrl Pts',(2.67602245442666,1.5704549653093,8.76439773149972));
#26857=CARTESIAN_POINT('Ctrl Pts',(1.95546857246677,2.4090594921577,8.8171953081955));
#26858=CARTESIAN_POINT('Ctrl Pts',(1.04734185348866,2.75437200587366,8.86999288489128));
#26859=CARTESIAN_POINT('Ctrl Pts',(0.139215134510575,3.09968451958961,8.92279046158706));
#26860=CARTESIAN_POINT('Ctrl Pts',(-0.956484421485707,2.95170502017316,
8.97558803828284));
#26861=CARTESIAN_POINT('Ctrl Pts',(-1.74047502001417,2.37786391736706,9.02838561497862));
#26862=CARTESIAN_POINT('Ctrl Pts',(-2.48014405062107,1.83646394008204,9.07819837095588));
#26863=CARTESIAN_POINT('Ctrl Pts',(-2.94235176373734,0.915992015346281,
9.12801112693314));
#26864=CARTESIAN_POINT('Ctrl Pts',(-2.94636616095733,-0.000987191619394096,
9.17782388291039));
#26865=CARTESIAN_POINT('Origin',(0.,0.,0.));
#26866=CARTESIAN_POINT('',(-2.94039988794905,0.00253112492490451,10.3221761170896));
#26867=CARTESIAN_POINT('',(-2.94130383534194,0.00264460613430074,10.1778238829104));
#26868=CARTESIAN_POINT('',(-2.942,-3.60291088309151E-16,0.));
#26869=CARTESIAN_POINT('Ctrl Pts',(-2.94039988794905,0.00253112492490451,
10.3221761170896));
#26870=CARTESIAN_POINT('Ctrl Pts',(-2.94274634020493,0.285190445035712,
10.3069016455741));
#26871=CARTESIAN_POINT('Ctrl Pts',(-2.90528029294341,0.56724066031149,10.2916271740585));
#26872=CARTESIAN_POINT('Ctrl Pts',(-2.82546634051429,0.836749725297203,
10.276352702543));
#26873=CARTESIAN_POINT('Ctrl Pts',(-2.54975713558759,1.76774146002846,10.2235885896398));
#26874=CARTESIAN_POINT('Ctrl Pts',(-1.76871589896699,2.54908128327144,10.1708244767365));
#26875=CARTESIAN_POINT('Ctrl Pts',(-0.837829613801701,2.82514631168034,
10.1180603638333));
#26876=CARTESIAN_POINT('Ctrl Pts',(0.0930566713635576,3.10121134008923,
10.0652962509301));
#26877=CARTESIAN_POINT('Ctrl Pts',(1.17378800507349,2.87200157366407,10.0125321380269));
#26878=CARTESIAN_POINT('Ctrl Pts',(1.91247496663932,2.24184068259591,9.95976802512365));
#26879=CARTESIAN_POINT('Ctrl Pts',(2.65116192820514,1.61167979152774,9.90700391222042));
#26880=CARTESIAN_POINT('Ctrl Pts',(3.04780451762686,0.580567775816567,9.8542397993172));
#26881=CARTESIAN_POINT('Ctrl Pts',(2.92187285902738,-0.382189926402199,
9.80147568641397));
#26882=CARTESIAN_POINT('Ctrl Pts',(2.79594120042789,-1.34494762862098,9.74871157351074));
#26883=CARTESIAN_POINT('Ctrl Pts',(2.14743529380718,-2.23935101734735,9.69594746060752));
#26884=CARTESIAN_POINT('Ctrl Pts',(1.27151933471594,-2.65831689713767,9.64318334770429));
#26885=CARTESIAN_POINT('Ctrl Pts',(0.395603375624702,-3.077282776928,9.59041923480107));
#26886=CARTESIAN_POINT('Ctrl Pts',(-0.707722635937064,-3.02081114778227,
9.53765512189783));
#26887=CARTESIAN_POINT('Ctrl Pts',(-1.53628542551181,-2.51460478714333,
9.48489100899461));
#26888=CARTESIAN_POINT('Ctrl Pts',(-2.36484821508653,-2.0083984265044,9.43212689609138));
#26889=CARTESIAN_POINT('Ctrl Pts',(-2.91864778267424,-1.05245733437228,
9.37936278318816));
#26890=CARTESIAN_POINT('Ctrl Pts',(-2.94562504570603,-0.0818732818047256,
9.32659867028494));
#26891=CARTESIAN_POINT('Ctrl Pts',(-2.94637876747043,-0.054755989597048,
9.32512448588649));
#26892=CARTESIAN_POINT('Ctrl Pts',(-2.9467212538342,-0.0276272671525533,
9.32365030148805));
#26893=CARTESIAN_POINT('Ctrl Pts',(-2.94665746643035,-0.000496894171833351,
9.3221761170896));
#26894=CARTESIAN_POINT('Ctrl Pts',(-2.94636616095733,-0.000987191619394096,
9.17782388291039));
#26895=CARTESIAN_POINT('Ctrl Pts',(-2.946606706893,-0.0559333290436887,
9.18080870362892));
#26896=CARTESIAN_POINT('Ctrl Pts',(-2.94520210810221,-0.110866925852438,
9.18379352434745));
#26897=CARTESIAN_POINT('Ctrl Pts',(-2.94211348083954,-0.165705674832853,
9.18677834506597));
#26898=CARTESIAN_POINT('Ctrl Pts',(-2.88747970207578,-1.13573145803076,
9.23957592176175));
#26899=CARTESIAN_POINT('Ctrl Pts',(-2.30593050348768,-2.07608031823082,
9.29237349845753));
#26900=CARTESIAN_POINT('Ctrl Pts',(-1.46246273194259,-2.55825973319532,
9.34517107515332));
#26901=CARTESIAN_POINT('Ctrl Pts',(-0.618994960397504,-3.04043914815982,
9.3979686518491));
#26902=CARTESIAN_POINT('Ctrl Pts',(0.486391384104583,-3.06444911788875,
9.45076622854488));
#26903=CARTESIAN_POINT('Ctrl Pts',(1.35000048945615,-2.61934892354526,9.50356380524066));
#26904=CARTESIAN_POINT('Ctrl Pts',(2.21360959480774,-2.17424872920176,9.55636138193644));
#26905=CARTESIAN_POINT('Ctrl Pts',(2.8354414610088,-1.26003837078583,9.60915895863223));
#26906=CARTESIAN_POINT('Ctrl Pts',(2.93214347709368,-0.293299734992319,
9.66195653532801));
#26907=CARTESIAN_POINT('Ctrl Pts',(3.02884549317855,0.673438900801169,9.71475411202378));
#26908=CARTESIAN_POINT('Ctrl Pts',(2.60041765914726,1.69270581397223,9.76755168871956));
#26909=CARTESIAN_POINT('Ctrl Pts',(1.84208339789187,2.30004757777328,9.82034926541534));
#26910=CARTESIAN_POINT('Ctrl Pts',(1.08374913663646,2.90738934157434,9.87314684211112));
#26911=CARTESIAN_POINT('Ctrl Pts',(-0.00449155184308325,3.10280595600537,
9.92594441880692));
#26912=CARTESIAN_POINT('Ctrl Pts',(-0.926755685023515,2.79725115159261,
9.9787419955027));
#26913=CARTESIAN_POINT('Ctrl Pts',(-1.84901981820395,2.49169634717984,10.0315395721985));
#26914=CARTESIAN_POINT('Ctrl Pts',(-2.60530739608529,1.6851701239233,10.0843371488943));
#26915=CARTESIAN_POINT('Ctrl Pts',(-2.85099783635035,0.745185508403901,
10.13713472559));
#26916=CARTESIAN_POINT('Ctrl Pts',(-2.91411270892398,0.503714944202581,
10.1506977780301));
#26917=CARTESIAN_POINT('Ctrl Pts',(-2.94353259565806,0.253437282769067,
10.1642608304703));
#26918=CARTESIAN_POINT('Ctrl Pts',(-2.94130383534194,0.00264460613430074,
10.1778238829104));
#26919=CARTESIAN_POINT('Origin',(0.,0.,0.));
#26920=CARTESIAN_POINT('',(-2.93811988821084,-0.00158572391977807,11.3221761170896));
#26921=CARTESIAN_POINT('',(-2.9376139453736,-0.001087489077759,11.1778238829104));
#26922=CARTESIAN_POINT('',(-2.942,-3.60291088309151E-16,0.));
#26923=CARTESIAN_POINT('Ctrl Pts',(-2.93811988821084,-0.00158572391977807,
11.3221761170896));
#26924=CARTESIAN_POINT('Ctrl Pts',(-2.93519577795759,0.592173285545134,
11.2901529896601));
#26925=CARTESIAN_POINT('Ctrl Pts',(-2.76052119328951,1.18751446039404,11.2581298622306));
#26926=CARTESIAN_POINT('Ctrl Pts',(-2.42602614988553,1.6726647196123,11.2261067348011));
#26927=CARTESIAN_POINT('Ctrl Pts',(-1.87488278406078,2.47204083016763,11.1733426218978));
#26928=CARTESIAN_POINT('Ctrl Pts',(-0.889846893775436,2.97226240860755,
11.1205785089946));
#26929=CARTESIAN_POINT('Ctrl Pts',(0.0807473991431609,2.94565612414208,
11.0678143960914));
#26930=CARTESIAN_POINT('Ctrl Pts',(1.05134169206174,2.91904983967661,11.0150502831882));
#26931=CARTESIAN_POINT('Ctrl Pts',(2.00749438761357,2.36561569230577,10.9622861702849));
#26932=CARTESIAN_POINT('Ctrl Pts',(2.51401740451069,1.53724644542814,10.9095220573817));
#26933=CARTESIAN_POINT('Ctrl Pts',(3.02054042140782,0.70887719855049,10.8567579444785));
#26934=CARTESIAN_POINT('Ctrl Pts',(3.07743375965022,-0.394427147833989,
10.8039938315753));
#26935=CARTESIAN_POINT('Ctrl Pts',(2.65880270302471,-1.27050318006396,10.751229718672));
#26936=CARTESIAN_POINT('Ctrl Pts',(2.2401716463992,-2.14657921229393,10.6984656057688));
#26937=CARTESIAN_POINT('Ctrl Pts',(1.34601619490581,-2.79542693036942,10.6457014928656));
#26938=CARTESIAN_POINT('Ctrl Pts',(0.383306696605943,-2.92172656497852,
10.5929373799624));
#26939=CARTESIAN_POINT('Ctrl Pts',(-0.579402801693943,-3.04802619958762,
10.5401732670591));
#26940=CARTESIAN_POINT('Ctrl Pts',(-1.6106663468003,-2.65177775073031,10.4874091541559));
#26941=CARTESIAN_POINT('Ctrl Pts',(-2.24110953273706,-1.91333170319189,
10.4346450412527));
#26942=CARTESIAN_POINT('Ctrl Pts',(-2.68904824819375,-1.38865544156027,
10.397155399865));
#26943=CARTESIAN_POINT('Ctrl Pts',(-2.93464075883505,-0.691227512489607,
10.3596657584773));
#26944=CARTESIAN_POINT('Ctrl Pts',(-2.94039988794905,0.00253112492490451,
10.3221761170896));
#26945=CARTESIAN_POINT('Ctrl Pts',(-2.94130383534194,0.00264460613430074,
10.1778238829104));
#26946=CARTESIAN_POINT('Ctrl Pts',(-2.93485658822933,-0.722835988887616,
10.217058407166));
#26947=CARTESIAN_POINT('Ctrl Pts',(-2.66357332332191,-1.45262623338011,
10.2562929314217));
#26948=CARTESIAN_POINT('Ctrl Pts',(-2.17698883749842,-1.98600345070618,
10.2955274556774));
#26949=CARTESIAN_POINT('Ctrl Pts',(-1.52219609573261,-2.70376478651468,
10.3483250323732));
#26950=CARTESIAN_POINT('Ctrl Pts',(-0.477517309552185,-3.06584445034943,
10.4011226090689));
#26951=CARTESIAN_POINT('Ctrl Pts',(0.481014564589377,-2.90725215512216,
10.4539201857647));
#26952=CARTESIAN_POINT('Ctrl Pts',(1.43954643873093,-2.7486598598949,10.5067177624605));
#26953=CARTESIAN_POINT('Ctrl Pts',(2.3119314008336,-2.06939560560563,10.5595153391563));
#26954=CARTESIAN_POINT('Ctrl Pts',(2.70064630965162,-1.17898244896802,10.6123129158521));
#26955=CARTESIAN_POINT('Ctrl Pts',(3.08936121846965,-0.288569292330407,
10.6651104925479));
#26956=CARTESIAN_POINT('Ctrl Pts',(2.99440607400299,0.812992766655582,10.7179080692436));
#26957=CARTESIAN_POINT('Ctrl Pts',(2.45904946631867,1.62375054334323,10.7707056459394));
#26958=CARTESIAN_POINT('Ctrl Pts',(1.92369285863434,2.43450832003088,10.8235032226352));
#26959=CARTESIAN_POINT('Ctrl Pts',(0.947934787732336,2.95446181442022,10.876300799331));
#26960=CARTESIAN_POINT('Ctrl Pts',(-0.023597167633587,2.94668174027824,
10.9290983760268));
#26961=CARTESIAN_POINT('Ctrl Pts',(-0.995129122999497,2.93890166613627,
10.9818959527225));
#26962=CARTESIAN_POINT('Ctrl Pts',(-1.96243496282931,2.40338802346302,11.0346935294183));
#26963=CARTESIAN_POINT('Ctrl Pts',(-2.48473857027235,1.58416045342967,11.0874911061141));
#26964=CARTESIAN_POINT('Ctrl Pts',(-2.78261294345243,1.11694771463552,11.1176020317129));
#26965=CARTESIAN_POINT('Ctrl Pts',(-2.93574936512043,0.557456399077179,
11.1477129573116));
#26966=CARTESIAN_POINT('Ctrl Pts',(-2.9376139453736,-0.001087489077759,
11.1778238829104));
#26967=CARTESIAN_POINT('Origin',(0.,0.,0.));
#26968=CARTESIAN_POINT('',(-2.9460560275736,-0.00128820797444335,12.3221761170896));
#26969=CARTESIAN_POINT('',(-2.94523166487087,-0.00185944496279741,12.1778238829104));
#26970=CARTESIAN_POINT('',(-2.942,-3.60291088309151E-16,0.));
#26971=CARTESIAN_POINT('Ctrl Pts',(-2.9460560275736,-0.00128820797444335,
12.3221761170896));
#26972=CARTESIAN_POINT('Ctrl Pts',(-2.94111144504364,0.896779189536789,
12.2734043337461));
#26973=CARTESIAN_POINT('Ctrl Pts',(-2.50046702038657,1.79904631809884,12.2246325504026));
#26974=CARTESIAN_POINT('Ctrl Pts',(-1.78678689418432,2.3432461968251,12.1758607670591));
#26975=CARTESIAN_POINT('Ctrl Pts',(-1.01468679502424,2.93199284241738,12.1230966541559));
#26976=CARTESIAN_POINT('Ctrl Pts',(0.0769784812166023,3.10165208129682,
12.0703325412527));
#26977=CARTESIAN_POINT('Ctrl Pts',(0.991342985003044,2.77500436580727,12.0175684283495));
#26978=CARTESIAN_POINT('Ctrl Pts',(1.90570748878951,2.4483566503177,11.9648043154462));
#26979=CARTESIAN_POINT('Ctrl Pts',(2.64277122012159,1.62540198045911,11.912040202543));
#26980=CARTESIAN_POINT('Ctrl Pts',(2.86706333577767,0.680704027315496,11.8592760896398));
#26981=CARTESIAN_POINT('Ctrl Pts',(3.09135545143376,-0.263993925828108,
11.8065119767365));
#26982=CARTESIAN_POINT('Ctrl Pts',(2.80287595141388,-1.33043516225671,11.7537478638333));
#26983=CARTESIAN_POINT('Ctrl Pts',(2.13292482649212,-2.03323432705079,11.7009837509301));
#26984=CARTESIAN_POINT('Ctrl Pts',(1.46297370157037,-2.73603349184485,11.6482196380269));
#26985=CARTESIAN_POINT('Ctrl Pts',(0.411550951746749,-3.07519058500439,
11.5954555251236));
#26986=CARTESIAN_POINT('Ctrl Pts',(-0.542793656558674,-2.89633996460426,
11.5426914122204));
#26987=CARTESIAN_POINT('Ctrl Pts',(-1.49713826486415,-2.71748934420412,
11.4899272993172));
#26988=CARTESIAN_POINT('Ctrl Pts',(-2.35440473165143,-2.02063101024426,
11.437163186414));
#26989=CARTESIAN_POINT('Ctrl Pts',(-2.72441254436296,-1.12293652192895,
11.3843990735107));
#26990=CARTESIAN_POINT('Ctrl Pts',(-2.86985849704456,-0.770062810659939,
11.363658088037));
#26991=CARTESIAN_POINT('Ctrl Pts',(-2.94001379842994,-0.386156125961379,
11.3429171025633));
#26992=CARTESIAN_POINT('Ctrl Pts',(-2.93811988821084,-0.00158572391977807,
11.3221761170896));
#26993=CARTESIAN_POINT('Ctrl Pts',(-2.9376139453736,-0.001087489077759,
11.1778238829104));
#26994=CARTESIAN_POINT('Ctrl Pts',(-2.93901878699851,-0.421914483298863,
11.2005105340074));
#26995=CARTESIAN_POINT('Ctrl Pts',(-2.85455180894317,-0.842203655580439,
11.2231971851044));
#26996=CARTESIAN_POINT('Ctrl Pts',(-2.68141846901601,-1.22208227989338,
11.2458838362014));
#26997=CARTESIAN_POINT('Ctrl Pts',(-2.27849338526037,-2.10615594578964,
11.2986814128972));
#26998=CARTESIAN_POINT('Ctrl Pts',(-1.39534184269282,-2.77136178018875,
11.351478989593));
#26999=CARTESIAN_POINT('Ctrl Pts',(-0.434393033296842,-2.91458278273799,
11.4042765662888));
#27000=CARTESIAN_POINT('Ctrl Pts',(0.526555776099161,-3.05780378528724,
11.4570741429846));
#27001=CARTESIAN_POINT('Ctrl Pts',(1.56530185232359,-2.6790399559866,11.5098717196804));
#27002=CARTESIAN_POINT('Ctrl Pts',(2.20851562057241,-1.95088412226283,11.5626692963761));
#27003=CARTESIAN_POINT('Ctrl Pts',(2.8517293888212,-1.22272828853909,11.6154668730719));
#27004=CARTESIAN_POINT('Ctrl Pts',(3.09941084909442,-0.145180450392246,
11.6682644497677));
#27005=CARTESIAN_POINT('Ctrl Pts',(2.83869800079219,0.790748863488276,11.7210620264635));
#27006=CARTESIAN_POINT('Ctrl Pts',(2.57798515248995,1.72667817736883,11.7738596031593));
#27007=CARTESIAN_POINT('Ctrl Pts',(1.80887799561223,2.52098896698305,11.8266571798551));
#27008=CARTESIAN_POINT('Ctrl Pts',(0.881838661257381,2.81173446120386,11.8794547565508));
#27009=CARTESIAN_POINT('Ctrl Pts',(-0.0452006730974654,3.10247995542467,
11.9322523332466));
#27010=CARTESIAN_POINT('Ctrl Pts',(-1.13017218492944,2.88966015425208,11.9850499099424));
#27011=CARTESIAN_POINT('Ctrl Pts',(-1.87868257050012,2.27025150679581,12.0378474866382));
#27012=CARTESIAN_POINT('Ctrl Pts',(-2.54016360114299,1.72286154613935,12.0845062853956));
#27013=CARTESIAN_POINT('Ctrl Pts',(-2.93887569608656,0.857934401938529,
12.131165084153));
#27014=CARTESIAN_POINT('Ctrl Pts',(-2.94523166487087,-0.00185944496279741,
12.1778238829104));
#27015=CARTESIAN_POINT('Origin',(0.,0.,0.));
#27016=CARTESIAN_POINT('',(-2.94174180320762,0.00264834375568943,13.3221761170896));
#27017=CARTESIAN_POINT('',(-2.94305001533088,0.00255625401320253,13.1778238829104));
#27018=CARTESIAN_POINT('',(-2.942,-3.60291088309151E-16,0.));
#27019=CARTESIAN_POINT('Ctrl Pts',(-2.94174180320762,0.00264834375568943,
13.3221761170896));
#27020=CARTESIAN_POINT('Ctrl Pts',(-2.94387102475549,0.238434505128271,
13.3094197907354));
#27021=CARTESIAN_POINT('Ctrl Pts',(-2.91788746839781,0.47375723479733,13.2966634643811));
#27022=CARTESIAN_POINT('Ctrl Pts',(-2.86198621303624,0.701744298554981,
13.2839071380269));
#27023=CARTESIAN_POINT('Ctrl Pts',(-2.63076132372094,1.64476933872116,13.2311430251236));
#27024=CARTESIAN_POINT('Ctrl Pts',(-1.88767285741819,2.4622880626259,13.1783789122204));
#27025=CARTESIAN_POINT('Ctrl Pts',(-0.970933785112477,2.78221094259426,
13.1256147993172));
#27026=CARTESIAN_POINT('Ctrl Pts',(-0.0541947128067906,3.10213382256261,
13.072850686414));
#27027=CARTESIAN_POINT('Ctrl Pts',(1.03619496550185,2.92446085859461,13.0200865735107));
#27028=CARTESIAN_POINT('Ctrl Pts',(1.80394988224929,2.33005900493893,12.9673224606075));
#27029=CARTESIAN_POINT('Ctrl Pts',(2.57170479899673,1.73565715128324,12.9145583477043));
#27030=CARTESIAN_POINT('Ctrl Pts',(3.01682495418297,0.724526407939868,12.8617942348011));
#27031=CARTESIAN_POINT('Ctrl Pts',(2.93671615215365,-0.243122162387507,
12.8090301218978));
#27032=CARTESIAN_POINT('Ctrl Pts',(2.85660735012433,-1.21077073271488,12.7562660089946));
#27033=CARTESIAN_POINT('Ctrl Pts',(2.25126959087945,-2.13493713002626,12.7035018960914));
#27034=CARTESIAN_POINT('Ctrl Pts',(1.39621930521764,-2.59499167549757,12.6507377831882));
#27035=CARTESIAN_POINT('Ctrl Pts',(0.541169019555798,-3.0550462209689,12.5979736702849));
#27036=CARTESIAN_POINT('Ctrl Pts',(-0.563593792522998,-3.05098891460014,
12.5452095573817));
#27037=CARTESIAN_POINT('Ctrl Pts',(-1.41524190404595,-2.58466641894008,
12.4924454444785));
#27038=CARTESIAN_POINT('Ctrl Pts',(-2.26689001556888,-2.11834392328004,
12.4396813315753));
#27039=CARTESIAN_POINT('Ctrl Pts',(-2.86542342653597,-1.18975623832874,
12.386917218672));
#27040=CARTESIAN_POINT('Ctrl Pts',(-2.93842267097986,-0.221545369700522,
12.3341531057688));
#27041=CARTESIAN_POINT('Ctrl Pts',(-2.94394606605647,-0.148286924552967,
12.3301607762091));
#27042=CARTESIAN_POINT('Ctrl Pts',(-2.94646077805926,-0.0748016366810879,
12.3261684466493));
#27043=CARTESIAN_POINT('Ctrl Pts',(-2.9460560275736,-0.00128820797444335,
12.3221761170896));
#27044=CARTESIAN_POINT('Ctrl Pts',(-2.94523166487087,-0.00185944496279741,
12.1778238829104));
#27045=CARTESIAN_POINT('Ctrl Pts',(-2.94606790330798,-0.11498030618232,
12.1839626608488));
#27046=CARTESIAN_POINT('Ctrl Pts',(-2.94011246232577,-0.228012310092633,
12.1901014387871));
#27047=CARTESIAN_POINT('Ctrl Pts',(-2.92707021611942,-0.34022059713689,
12.1962402167255));
#27048=CARTESIAN_POINT('Ctrl Pts',(-2.81489821685867,-1.30528655987343,
12.2490377934213));
#27049=CARTESIAN_POINT('Ctrl Pts',(-2.17850495902776,-2.20942099160657,
12.3018353701171));
#27050=CARTESIAN_POINT('Ctrl Pts',(-1.30787830109555,-2.64063334341081,
12.3546329468129));
#27051=CARTESIAN_POINT('Ctrl Pts',(-0.437251643163329,-3.07184569521506,
12.4074305235086));
#27052=CARTESIAN_POINT('Ctrl Pts',(0.667608414870202,-3.0301359670904,12.4602281002044));
#27053=CARTESIAN_POINT('Ctrl Pts',(1.50324587595541,-2.53451019750022,12.5130256769002));
#27054=CARTESIAN_POINT('Ctrl Pts',(2.3388833370406,-2.03888442791006,12.565823253596));
#27055=CARTESIAN_POINT('Ctrl Pts',(2.90529820117748,-1.0893426168544,12.6186208302918));
#27056=CARTESIAN_POINT('Ctrl Pts',(2.94438994414644,-0.118566275217254,
12.6714184069876));
#27057=CARTESIAN_POINT('Ctrl Pts',(2.9834816871154,0.852210066419907,12.7242159836833));
#27058=CARTESIAN_POINT('Ctrl Pts',(2.49525030891641,1.84422093863856,12.7770135603791));
#27059=CARTESIAN_POINT('Ctrl Pts',(1.70217015235411,2.40543278377184,12.8298111370749));
#27060=CARTESIAN_POINT('Ctrl Pts',(0.909089995791835,2.9666446289051,12.8826087137707));
#27061=CARTESIAN_POINT('Ctrl Pts',(-0.188838939133739,3.09705744695301,
12.9354062904664));
#27062=CARTESIAN_POINT('Ctrl Pts',(-1.09131898793251,2.7372455080587,12.9882038671622));
#27063=CARTESIAN_POINT('Ctrl Pts',(-1.99379903673132,2.37743356916437,13.041001443858));
#27064=CARTESIAN_POINT('Ctrl Pts',(-2.70083019940331,1.52739687332778,13.0937990205538));
#27065=CARTESIAN_POINT('Ctrl Pts',(-2.89023676115095,0.574475038014031,
13.1465965972496));
#27066=CARTESIAN_POINT('Ctrl Pts',(-2.92757845484148,0.386605542063277,
13.1570056924699));
#27067=CARTESIAN_POINT('Ctrl Pts',(-2.94480084734965,0.194737053204087,
13.1674147876901));
#27068=CARTESIAN_POINT('Ctrl Pts',(-2.94305001533088,0.00255625401320253,
13.1778238829104));
#27069=CARTESIAN_POINT('Origin',(0.,0.,0.));
#27070=CARTESIAN_POINT('',(-2.93751466932027,-0.000920155716999105,14.3221761170896));
#27071=CARTESIAN_POINT('',(-2.93723567126517,-0.000168200420414877,14.1778238829104));
#27072=CARTESIAN_POINT('',(-2.942,-3.60291088309151E-16,0.));
#27073=CARTESIAN_POINT('Ctrl Pts',(-2.93751466932027,-0.000920155716999105,
14.3221761170896));
#27074=CARTESIAN_POINT('Ctrl Pts',(-2.93597025204609,0.546430712607314,
14.2926711348214));
#27075=CARTESIAN_POINT('Ctrl Pts',(-2.78929401088964,1.09455044560389,14.2631661525532));
#27076=CARTESIAN_POINT('Ctrl Pts',(-2.50265848527962,1.55567048253069,14.2336611702849));
#27077=CARTESIAN_POINT('Ctrl Pts',(-1.99006474440319,2.38029696320978,14.1808970573817));
#27078=CARTESIAN_POINT('Ctrl Pts',(-1.02987285703515,2.92669322244838,14.1281329444785));
#27079=CARTESIAN_POINT('Ctrl Pts',(-0.0591093222587219,2.94616975617191,
14.0753688315753));
#27080=CARTESIAN_POINT('Ctrl Pts',(0.91165421251771,2.96564628989543,14.022604718672));
#27081=CARTESIAN_POINT('Ctrl Pts',(1.89298939470253,2.45820309810388,13.9698406057688));
#27082=CARTESIAN_POINT('Ctrl Pts',(2.43824646110908,1.6548003925117,13.9170764928656));
#27083=CARTESIAN_POINT('Ctrl Pts',(2.98350352751563,0.851397686919529,13.8643123799624));
#27084=CARTESIAN_POINT('Ctrl Pts',(3.09268247814392,-0.247964532473289,
13.8115482670591));
#27085=CARTESIAN_POINT('Ctrl Pts',(2.71609106377438,-1.14291709123984,13.7587841541559));
#27086=CARTESIAN_POINT('Ctrl Pts',(2.33949964940482,-2.03786965000643,13.7060200412527));
#27087=CARTESIAN_POINT('Ctrl Pts',(1.47713787003741,-2.72841254814676,13.6532559283495));
#27088=CARTESIAN_POINT('Ctrl Pts',(0.521505344074129,-2.90024866524679,
13.6004918154462));
#27089=CARTESIAN_POINT('Ctrl Pts',(-0.434127181889136,-3.07208478234682,
13.547727702543));
#27090=CARTESIAN_POINT('Ctrl Pts',(-1.48303045444825,-2.72521411840656,
13.4949635896398));
#27091=CARTESIAN_POINT('Ctrl Pts',(-2.14780143456386,-2.01751310822262,
13.4421994767365));
#27092=CARTESIAN_POINT('Ctrl Pts',(-2.65185644493049,-1.48090689240571,
13.4021916901876));
#27093=CARTESIAN_POINT('Ctrl Pts',(-2.93506390560319,-0.736850015994192,
13.3621839036386));
#27094=CARTESIAN_POINT('Ctrl Pts',(-2.94174180320762,0.00264834375568943,
13.3221761170896));
#27095=CARTESIAN_POINT('Ctrl Pts',(-2.94305001533088,0.00255625401320253,
13.1778238829104));
#27096=CARTESIAN_POINT('Ctrl Pts',(-2.93592018233154,-0.780052807971912,
13.2202123643859));
#27097=CARTESIAN_POINT('Ctrl Pts',(-2.61415254645348,-1.56784099153657,
13.2626008458614));
#27098=CARTESIAN_POINT('Ctrl Pts',(-2.05514306890902,-2.111842103739,13.3049893273369));
#27099=CARTESIAN_POINT('Ctrl Pts',(-1.35886085409615,-2.78943043538737,
13.3577869040327));
#27100=CARTESIAN_POINT('Ctrl Pts',(-0.294514463647097,-3.08880012389325,
13.4105844807285));
#27101=CARTESIAN_POINT('Ctrl Pts',(0.652901130166797,-2.87353618718061,
13.4633820574243));
#27102=CARTESIAN_POINT('Ctrl Pts',(1.60031672398072,-2.65827225046796,13.5161796341201));
#27103=CARTESIAN_POINT('Ctrl Pts',(2.43080152115949,-1.92837468853676,13.5689772108158));
#27104=CARTESIAN_POINT('Ctrl Pts',(2.76592519601784,-1.01643883969637,13.6217747875116));
#27105=CARTESIAN_POINT('Ctrl Pts',(3.10104887087618,-0.104502990856014,
13.6745723642074));
#27106=CARTESIAN_POINT('Ctrl Pts',(2.94081142341417,0.989471144893501,13.7273699409032));
#27107=CARTESIAN_POINT('Ctrl Pts',(2.35822889153647,1.7669880022038,13.780167517599));
#27108=CARTESIAN_POINT('Ctrl Pts',(1.77564635965879,2.54450485951408,13.8329650942947));
#27109=CARTESIAN_POINT('Ctrl Pts',(0.770718743365416,3.00556443838513,13.8857626709905));
#27110=CARTESIAN_POINT('Ctrl Pts',(-0.198634575296267,2.94007387837555,
13.9385602476863));
#27111=CARTESIAN_POINT('Ctrl Pts',(-1.16798789395799,2.87458331836597,13.9913578243821));
#27112=CARTESIAN_POINT('Ctrl Pts',(-2.10176691498804,2.28254261947571,14.0441554010779));
#27113=CARTESIAN_POINT('Ctrl Pts',(-2.57447282101243,1.43372933243287,14.0969529777737));
#27114=CARTESIAN_POINT('Ctrl Pts',(-2.81582325712524,1.00034896972683,14.1239099461526));
#27115=CARTESIAN_POINT('Ctrl Pts',(-2.9369793805535,0.500032141317613,14.1508669145315));
#27116=CARTESIAN_POINT('Ctrl Pts',(-2.93723567126517,-0.000168200420414877,
14.1778238829104));
#27117=CARTESIAN_POINT('Origin',(0.,0.,0.));
#27118=CARTESIAN_POINT('',(-2.94505309192038,-0.00193896756046696,15.3221761170896));
#27119=CARTESIAN_POINT('',(-2.94366018875525,-0.00243623744087094,15.1778238829104));
#27120=CARTESIAN_POINT('',(-2.942,-3.60291088309151E-16,0.));
#27121=CARTESIAN_POINT('Ctrl Pts',(-2.94505309192038,-0.00193896756046696,
15.3221761170896));
#27122=CARTESIAN_POINT('Ctrl Pts',(-2.9385470358389,0.850524388417163,15.2759224789074));
#27123=CARTESIAN_POINT('Ctrl Pts',(-2.547538609851,1.70819207565318,15.2296688407252));
#27124=CARTESIAN_POINT('Ctrl Pts',(-1.89595701623,2.25582737299276,15.183415202543));
#27125=CARTESIAN_POINT('Ctrl Pts',(-1.15266143727356,2.88054559612564,15.1306510896398));
#27126=CARTESIAN_POINT('Ctrl Pts',(-0.0702757065020065,3.101811187844,15.0778869767365));
#27127=CARTESIAN_POINT('Ctrl Pts',(0.858557765212819,2.81891622927623,15.0251228638333));
#27128=CARTESIAN_POINT('Ctrl Pts',(1.78739123692767,2.53602127070844,14.9723587509301));
#27129=CARTESIAN_POINT('Ctrl Pts',(2.56267244958579,1.74896576185448,14.9195946380269));
#27130=CARTESIAN_POINT('Ctrl Pts',(2.83153606576082,0.815974051442588,14.8668305251236));
#27131=CARTESIAN_POINT('Ctrl Pts',(3.10039968193584,-0.11701765896928,14.8140664122204));
#27132=CARTESIAN_POINT('Ctrl Pts',(2.86284570162781,-1.19594557093908,14.7613022993172));
#27133=CARTESIAN_POINT('Ctrl Pts',(2.22699562201281,-1.92974108203173,14.708538186414));
#27134=CARTESIAN_POINT('Ctrl Pts',(1.59114554239781,-2.66353659312438,14.6557740735107));
#27135=CARTESIAN_POINT('Ctrl Pts',(0.556999363475848,-3.05219970333988,
14.6030099606075));
#27136=CARTESIAN_POINT('Ctrl Pts',(-0.404756492565064,-2.91883235658634,
14.5502458477043));
#27137=CARTESIAN_POINT('Ctrl Pts',(-1.36651234860599,-2.78546500983279,
14.4974817348011));
#27138=CARTESIAN_POINT('Ctrl Pts',(-2.25587788176586,-2.13006720611019,
14.4447176218978));
#27139=CARTESIAN_POINT('Ctrl Pts',(-2.66806285115338,-1.25093995318909,
14.3919535089946));
#27140=CARTESIAN_POINT('Ctrl Pts',(-2.84975952946865,-0.86340883600752,
14.3686943783596));
#27141=CARTESIAN_POINT('Ctrl Pts',(-2.93873215194095,-0.432403395862752,
14.3454352477246));
#27142=CARTESIAN_POINT('Ctrl Pts',(-2.93751466932027,-0.000920155716999105,
14.3221761170896));
#27143=CARTESIAN_POINT('Ctrl Pts',(-2.93723567126517,-0.000168200420414877,
14.1778238829104));
#27144=CARTESIAN_POINT('Ctrl Pts',(-2.93748134829393,-0.479653909982754,
14.2036644912273));
#27145=CARTESIAN_POINT('Ctrl Pts',(-2.82663341825378,-0.959032581146549,
14.2295050995441));
#27146=CARTESIAN_POINT('Ctrl Pts',(-2.6040704337075,-1.37924156009726,14.255345707861));
#27147=CARTESIAN_POINT('Ctrl Pts',(-2.14932934935944,-2.23781329038918,
14.3081432845568));
#27148=CARTESIAN_POINT('Ctrl Pts',(-1.22821438964454,-2.84937087577762,
14.3609408612526));
#27149=CARTESIAN_POINT('Ctrl Pts',(-0.260453688517605,-2.9352434278857,
14.4137384379483));
#27150=CARTESIAN_POINT('Ctrl Pts',(0.707307012609348,-3.02111597999379,
14.4665360146441));
#27151=CARTESIAN_POINT('Ctrl Pts',(1.72171345514836,-2.58130349882152,14.5193335913399));
#27152=CARTESIAN_POINT('Ctrl Pts',(2.32052700242268,-1.81621709490922,14.5721311680357));
#27153=CARTESIAN_POINT('Ctrl Pts',(2.91934054969697,-1.05113069099694,14.6249287447315));
#27154=CARTESIAN_POINT('Ctrl Pts',(3.10256120170658,0.0392296356553336,
14.6777263214272));
#27155=CARTESIAN_POINT('Ctrl Pts',(2.78670007190605,0.958015038527095,14.730523898123));
#27156=CARTESIAN_POINT('Ctrl Pts',(2.4708389421055,1.87680044139888,14.7833214748188));
#27157=CARTESIAN_POINT('Ctrl Pts',(1.65589603049478,2.62401092049012,14.8361190515146));
#27158=CARTESIAN_POINT('Ctrl Pts',(0.713219629658999,2.85916209136071,14.8889166282104));
#27159=CARTESIAN_POINT('Ctrl Pts',(-0.229456771176758,3.09431326223129,
14.9417142049061));
#27160=CARTESIAN_POINT('Ctrl Pts',(-1.2998666612376,2.81740512488122,14.9945117816019));
#27161=CARTESIAN_POINT('Ctrl Pts',(-2.0102520891451,2.15461751661924,15.0473093582977));
#27162=CARTESIAN_POINT('Ctrl Pts',(-2.59560481564969,1.60848506746078,15.0908141998353));
#27163=CARTESIAN_POINT('Ctrl Pts',(-2.93651363712562,0.800354074714661,
15.1343190413728));
#27164=CARTESIAN_POINT('Ctrl Pts',(-2.94366018875525,-0.00243623744087094,
15.1778238829104));
#27165=CARTESIAN_POINT('Origin',(0.,0.,0.));
#27166=CARTESIAN_POINT('',(-2.94313738502513,0.00253302137586425,16.3221761170896));
#27167=CARTESIAN_POINT('',(-2.94471111638464,0.00210180365940244,16.1778238829104));
#27168=CARTESIAN_POINT('',(-2.942,-3.60291088309151E-16,0.));
#27169=CARTESIAN_POINT('Ctrl Pts',(-2.94313738502513,0.00253302137586425,
16.3221761170896));
#27170=CARTESIAN_POINT('Ctrl Pts',(-2.94485185925312,0.191543887392068,
16.3119379358966));
#27171=CARTESIAN_POINT('Ctrl Pts',(-2.9281926935312,0.380253813087586,16.3016997547037));
#27172=CARTESIAN_POINT('Ctrl Pts',(-2.89205921107313,0.565158123055661,
16.2914615735107));
#27173=CARTESIAN_POINT('Ctrl Pts',(-2.70583949957629,1.51809221394305,16.2386974606075));
#27174=CARTESIAN_POINT('Ctrl Pts',(-2.00237766161548,2.36994831590605,16.1859333477043));
#27175=CARTESIAN_POINT('Ctrl Pts',(-1.10185083601191,2.73300839513725,16.1331692348011));
#27176=CARTESIAN_POINT('Ctrl Pts',(-0.201324010408316,3.09606847436846,
16.0804051218978));
#27177=CARTESIAN_POINT('Ctrl Pts',(0.896267802838059,2.97033253086785,16.0276410089946));
#27178=CARTESIAN_POINT('Ctrl Pts',(1.69136123542551,2.41302865700962,15.9748768960914));
#27179=CARTESIAN_POINT('Ctrl Pts',(2.48645466801294,1.85572478315141,15.9221127831882));
#27180=CARTESIAN_POINT('Ctrl Pts',(2.97904971994149,0.866852978935614,15.8693486702849));
#27181=CARTESIAN_POINT('Ctrl Pts',(2.94494422784077,-0.103506742820716,
15.8165845573817));
#27182=CARTESIAN_POINT('Ctrl Pts',(2.91083873574005,-1.07386646457706,15.7638204444785));
#27183=CARTESIAN_POINT('Ctrl Pts',(2.35003269961009,-2.0257141038739,15.7110563315753));
#27184=CARTESIAN_POINT('Ctrl Pts',(1.51777416489894,-2.52582100099134,15.658292218672));
#27185=CARTESIAN_POINT('Ctrl Pts',(0.685515630187792,-3.02592789810876,
15.6055281057688));
#27186=CARTESIAN_POINT('Ctrl Pts',(-0.418195403104536,-3.07429405304675,
15.5527639928656));
#27187=CARTESIAN_POINT('Ctrl Pts',(-1.2910104219294,-2.64890585572412,15.4999998799623));
#27188=CARTESIAN_POINT('Ctrl Pts',(-2.16382544075429,-2.22351765840148,
15.4472357670591));
#27189=CARTESIAN_POINT('Ctrl Pts',(-2.80574444511171,-1.3243751088182,15.3944716541559));
#27190=CARTESIAN_POINT('Ctrl Pts',(-2.92460123371974,-0.360718406752851,
15.3417075412527));
#27191=CARTESIAN_POINT('Ctrl Pts',(-2.93926677200092,-0.241814434842101,
15.3351970665317));
#27192=CARTESIAN_POINT('Ctrl Pts',(-2.94596885801613,-0.121928255923654,
15.3286865918106));
#27193=CARTESIAN_POINT('Ctrl Pts',(-2.94505309192038,-0.00193896756046696,
15.3221761170896));
#27194=CARTESIAN_POINT('Ctrl Pts',(-2.94366018875525,-0.00243623744087094,
15.1778238829104));
#27195=CARTESIAN_POINT('Ctrl Pts',(-2.94518670877559,-0.173914111966714,
15.1871166180686));
#27196=CARTESIAN_POINT('Ctrl Pts',(-2.93148500754538,-0.345148312857129,
15.1964093532268));
#27197=CARTESIAN_POINT('Ctrl Pts',(-2.90168460531916,-0.513533403029899,
15.2057020883851));
#27198=CARTESIAN_POINT('Ctrl Pts',(-2.7323707278315,-1.47022963524309,15.2584996650808));
#27199=CARTESIAN_POINT('Ctrl Pts',(-2.04338200710198,-2.33495502049558,
15.3112972417766));
#27200=CARTESIAN_POINT('Ctrl Pts',(-1.14867268627487,-2.7136766875585,15.3640948184724));
#27201=CARTESIAN_POINT('Ctrl Pts',(-0.25396336544776,-3.09239835462142,
15.4168923951682));
#27202=CARTESIAN_POINT('Ctrl Pts',(0.846466555476943,-2.98511630349478,
15.469689971864));
#27203=CARTESIAN_POINT('Ctrl Pts',(1.65117977763893,-2.44071617499708,15.5224875485597));
#27204=CARTESIAN_POINT('Ctrl Pts',(2.45589299980093,-1.89631604649936,15.5752851252555));
#27205=CARTESIAN_POINT('Ctrl Pts',(2.9648895232002,-0.914797840630574,15.6280827019513));
#27206=CARTESIAN_POINT('Ctrl Pts',(2.94623286851971,0.0565861200307141,
15.6808802786471));
#27207=CARTESIAN_POINT('Ctrl Pts',(2.92757621383922,1.02797008069197,15.7336778553429));
#27208=CARTESIAN_POINT('Ctrl Pts',(2.38126638107898,1.98921979614572,15.7864754320387));
#27209=CARTESIAN_POINT('Ctrl Pts',(1.55624255416387,2.50231876814311,15.8392730087344));
#27210=CARTESIAN_POINT('Ctrl Pts',(0.731218727248764,3.01541774014049,15.8920705854302));
#27211=CARTESIAN_POINT('Ctrl Pts',(-0.372519093821215,3.08036596868152,
15.944868162126));
#27212=CARTESIAN_POINT('Ctrl Pts',(-1.25202628558859,2.66756823456797,15.9976657388218));
#27213=CARTESIAN_POINT('Ctrl Pts',(-2.13153347735599,2.2547705004544,16.0504633155176));
#27214=CARTESIAN_POINT('Ctrl Pts',(-2.78681003982076,1.36422680368623,16.1032608922133));
#27215=CARTESIAN_POINT('Ctrl Pts',(-2.91926348480717,0.401734749454156,
16.1560584689091));
#27216=CARTESIAN_POINT('Ctrl Pts',(-2.93746447209008,0.269474651268154,
16.1633136069095));
#27217=CARTESIAN_POINT('Ctrl Pts',(-2.94579316360478,0.135855976077432,
16.17056874491));
#27218=CARTESIAN_POINT('Ctrl Pts',(-2.94471111638464,0.00210180365940244,
16.1778238829104));
#27219=CARTESIAN_POINT('Origin',(0.,0.,0.));
#27220=CARTESIAN_POINT('',(-2.93725002901676,-0.0001812803941037,17.3221761170896));
#27221=CARTESIAN_POINT('',(-2.93741720373741,0.000771801339816214,17.1778238829104));
#27222=CARTESIAN_POINT('',(-2.942,-3.60291088309151E-16,0.));
#27223=CARTESIAN_POINT('Ctrl Pts',(-2.93725002901676,-0.0001812803941037,
17.3221761170896));
#27224=CARTESIAN_POINT('Ctrl Pts',(-2.93697279781615,0.500567342066419,
17.2951892799827));
#27225=CARTESIAN_POINT('Ctrl Pts',(-2.81551854411511,1.00144216616236,17.2682024428757));
#27226=CARTESIAN_POINT('Ctrl Pts',(-2.57365375306511,1.43517165229615,17.2412156057688));
#27227=CARTESIAN_POINT('Ctrl Pts',(-2.10076465191889,2.28319068784079,17.1884514928656));
#27228=CARTESIAN_POINT('Ctrl Pts',(-1.16757891458186,2.87453141365988,17.1356873799624));
#27229=CARTESIAN_POINT('Ctrl Pts',(-0.198832686731451,2.94004703408661,
17.0829232670591));
#27230=CARTESIAN_POINT('Ctrl Pts',(0.769913541118934,3.00556265451333,17.0301591541559));
#27231=CARTESIAN_POINT('Ctrl Pts',(1.7742202594827,2.54525316954771,16.9773950412527));
#27232=CARTESIAN_POINT('Ctrl Pts',(2.35698303829202,1.76862666853625,16.9246309283495));
#27233=CARTESIAN_POINT('Ctrl Pts',(2.93974581710134,0.992000167524792,16.8718668154462));
#27234=CARTESIAN_POINT('Ctrl Pts',(3.1009646563562,-0.10094334953251,16.819102702543));
#27235=CARTESIAN_POINT('Ctrl Pts',(2.76726124086461,-1.01275643457747,16.7663385896398));
#27236=CARTESIAN_POINT('Ctrl Pts',(2.43355782537301,-1.92456951962244,16.7135744767365));
#27237=CARTESIAN_POINT('Ctrl Pts',(1.60493215513494,-2.65525217265506,16.6608103638333));
#27238=CARTESIAN_POINT('Ctrl Pts',(0.658529223760488,-2.87223771613265,
16.6080462509301));
#27239=CARTESIAN_POINT('Ctrl Pts',(-0.28787370761399,-3.08922325961025,
16.5552821380269));
#27240=CARTESIAN_POINT('Ctrl Pts',(-1.35205390012486,-2.79251169353279,
16.5025180251236));
#27241=CARTESIAN_POINT('Ctrl Pts',(-2.04965520386386,-2.11714987058814,
16.4497539122204));
#27242=CARTESIAN_POINT('Ctrl Pts',(-2.61189616218738,-1.57283311471008,
16.4072279805101));
#27243=CARTESIAN_POINT('Ctrl Pts',(-2.93601604066088,-0.782554000353691,
16.3647020487999));
#27244=CARTESIAN_POINT('Ctrl Pts',(-2.94313738502513,0.00253302137586425,
16.3221761170896));
#27245=CARTESIAN_POINT('Ctrl Pts',(-2.94471111638464,0.00210180365940244,
16.1778238829104));
#27246=CARTESIAN_POINT('Ctrl Pts',(-2.93791881702584,-0.837508855329917,
16.2233663216058));
#27247=CARTESIAN_POINT('Ctrl Pts',(-2.56030500077532,-1.68245865812038,
16.2689087603011));
#27248=CARTESIAN_POINT('Ctrl Pts',(-1.9260357734749,-2.23021889165449,16.3144511989965));
#27249=CARTESIAN_POINT('Ctrl Pts',(-1.19072428964819,-2.86524006683513,
16.3672487756922));
#27250=CARTESIAN_POINT('Ctrl Pts',(-0.110470994486742,-3.10084200550047,
16.420046352388));
#27251=CARTESIAN_POINT('Ctrl Pts',(0.822480772671947,-2.82966702812486,
16.4728439290838));
#27252=CARTESIAN_POINT('Ctrl Pts',(1.75543253983062,-2.55849205074926,16.5256415057796));
#27253=CARTESIAN_POINT('Ctrl Pts',(2.54108277898654,-1.78054015733275,16.5784390824754));
#27254=CARTESIAN_POINT('Ctrl Pts',(2.82143111474126,-0.850303800757864,
16.6312366591711));
#27255=CARTESIAN_POINT('Ctrl Pts',(3.10177945049598,0.0799325558170201,
16.6840342358669));
#27256=CARTESIAN_POINT('Ctrl Pts',(2.8768258828495,1.16245337555027,16.7368318125627));
#27257=CARTESIAN_POINT('Ctrl Pts',(2.24907588729453,1.90398208157484,16.7896293892585));
#27258=CARTESIAN_POINT('Ctrl Pts',(1.62132589173955,2.64551078759941,16.8424269659543));
#27259=CARTESIAN_POINT('Ctrl Pts',(0.590779468276065,3.0460473799153,16.8952245426501));
#27260=CARTESIAN_POINT('Ctrl Pts',(-0.372970147291156,2.92307772968038,
16.9480221193458));
#27261=CARTESIAN_POINT('Ctrl Pts',(-1.33671976285836,2.80010807944546,17.0008196960416));
#27262=CARTESIAN_POINT('Ctrl Pts',(-2.23367257052931,2.15363218665976,17.0536172727374));
#27263=CARTESIAN_POINT('Ctrl Pts',(-2.65511055711324,1.27823234158675,17.1064148494332));
#27264=CARTESIAN_POINT('Ctrl Pts',(-2.84510967687048,0.883571192629371,
17.1302178605922));
#27265=CARTESIAN_POINT('Ctrl Pts',(-2.93845923718072,0.442380686112001,
17.1540208717513));
#27266=CARTESIAN_POINT('Ctrl Pts',(-2.93741720373741,0.000771801339816214,
17.1778238829104));
#27267=CARTESIAN_POINT('Origin',(0.,0.,0.));
#27268=CARTESIAN_POINT('',(-2.94374845943093,-0.00235935217182681,18.3221761170896));
#27269=CARTESIAN_POINT('',(-2.94191884508495,-0.00265442804262754,18.1778238829104));
#27270=CARTESIAN_POINT('',(-2.942,-3.60291088309151E-16,0.));
#27271=CARTESIAN_POINT('Ctrl Pts',(-2.94374845943093,-0.00235935217182681,
18.3221761170896));
#27272=CARTESIAN_POINT('Ctrl Pts',(-2.93663601505887,0.804593723390554,
18.2784406240687));
#27273=CARTESIAN_POINT('Ctrl Pts',(-2.59170604511532,1.61685233182154,18.2347051310478));
#27274=CARTESIAN_POINT('Ctrl Pts',(-2.00087556349472,2.16331231972268,18.1909696380269));
#27275=CARTESIAN_POINT('Ctrl Pts',(-1.28807586499836,2.82258181703745,18.1382055251236));
#27276=CARTESIAN_POINT('Ctrl Pts',(-0.21737042847422,3.09498407768528,18.0854414122204));
#27277=CARTESIAN_POINT('Ctrl Pts',(0.723848642366025,2.85648596639017,18.0326772993172));
#27278=CARTESIAN_POINT('Ctrl Pts',(1.66506771320627,2.61798785509506,17.979913186414));
#27279=CARTESIAN_POINT('Ctrl Pts',(2.47680041836259,1.86858937185697,17.9271490735107));
#27280=CARTESIAN_POINT('Ctrl Pts',(2.78962522811136,0.949401968316567,17.8743849606075));
#27281=CARTESIAN_POINT('Ctrl Pts',(3.10245003786014,0.0302145647761227,
17.8216208477043));
#27282=CARTESIAN_POINT('Ctrl Pts',(2.91636695220134,-1.05876175906663,17.7688567348011));
#27283=CARTESIAN_POINT('Ctrl Pts',(2.31605267190429,-1.82189879882254,17.7160926218978));
#27284=CARTESIAN_POINT('Ctrl Pts',(1.71573839160727,-2.58503583857842,17.6633285089946));
#27285=CARTESIAN_POINT('Ctrl Pts',(0.701192916672019,-3.02233359424745,
17.6105643960914));
#27286=CARTESIAN_POINT('Ctrl Pts',(-0.26580902510543,-2.93475092606069,
17.5578002831882));
#27287=CARTESIAN_POINT('Ctrl Pts',(-1.23281096688288,-2.84716825787392,
17.5050361702849));
#27288=CARTESIAN_POINT('Ctrl Pts',(-2.15226937550254,-2.23470516583136,
17.4522720573817));
#27289=CARTESIAN_POINT('Ctrl Pts',(-2.60570234733465,-1.376124947175,17.3995079444785));
#27290=CARTESIAN_POINT('Ctrl Pts',(-2.82722159833554,-0.956675858167516,
17.3737306686822));
#27291=CARTESIAN_POINT('Ctrl Pts',(-2.93751483459916,-0.478486140449837,
17.3479533928859));
#27292=CARTESIAN_POINT('Ctrl Pts',(-2.93725002901676,-0.0001812803941037,
17.3221761170896));
#27293=CARTESIAN_POINT('Ctrl Pts',(-2.93741720373741,0.000771801339816214,
17.1778238829104));
#27294=CARTESIAN_POINT('Ctrl Pts',(-2.93614789764997,-0.537154163806018,
17.2068184484471));
#27295=CARTESIAN_POINT('Ctrl Pts',(-2.79482226555546,-1.07570091009264,
17.2358130139838));
#27296=CARTESIAN_POINT('Ctrl Pts',(-2.51752135312617,-1.53152748460635,
17.2648075795205));
#27297=CARTESIAN_POINT('Ctrl Pts',(-2.01257099705827,-2.36156366836612,
17.3176051562163));
#27298=CARTESIAN_POINT('Ctrl Pts',(-1.05674711942554,-2.91731223852532,
17.3704027329121));
#27299=CARTESIAN_POINT('Ctrl Pts',(-0.0855940111972479,-2.94553288784212,
17.4232003096079));
#27300=CARTESIAN_POINT('Ctrl Pts',(0.885559097031044,-2.97375353715892,
17.4759978863037));
#27301=CARTESIAN_POINT('Ctrl Pts',(1.87204143585492,-2.47444626563332,17.5287954629994));
#27302=CARTESIAN_POINT('Ctrl Pts',(2.42433904935325,-1.6751326720045,17.5815930396952));
#27303=CARTESIAN_POINT('Ctrl Pts',(2.97663666285158,-0.875819078375684,
17.634390616391));
#27304=CARTESIAN_POINT('Ctrl Pts',(3.09474955102439,0.223500837356317,17.6871881930868));
#27305=CARTESIAN_POINT('Ctrl Pts',(2.72485599198232,1.12189607224172,17.7399857697826));
#27306=CARTESIAN_POINT('Ctrl Pts',(2.35496243294025,2.02029130712709,17.7927833464783));
#27307=CARTESIAN_POINT('Ctrl Pts',(1.49706242668327,2.71776186116588,17.8455809231741));
#27308=CARTESIAN_POINT('Ctrl Pts',(0.542080129465371,2.89648759437067,17.8983784998699));
#27309=CARTESIAN_POINT('Ctrl Pts',(-0.412902167752565,3.07521332757547,
17.9511760765657));
#27310=CARTESIAN_POINT('Ctrl Pts',(-1.46496675593142,2.73519423994629,18.0039736532615));
#27311=CARTESIAN_POINT('Ctrl Pts',(-2.13471789678605,2.03136999411808,18.0567712299573));
#27312=CARTESIAN_POINT('Ctrl Pts',(-2.64657947259283,1.49346783078479,18.097122114275));
#27313=CARTESIAN_POINT('Ctrl Pts',(-2.93513642830927,0.743071513225126,
18.1374729985927));
#27314=CARTESIAN_POINT('Ctrl Pts',(-2.94191884508495,-0.00265442804262754,
18.1778238829104));
#27315=CARTESIAN_POINT('Origin',(0.,0.,-1.84858989190501));
#27316=CARTESIAN_POINT('',(-2.37315955426761,-0.00190203722427915,18.651410108095));
#27317=CARTESIAN_POINT('',(-2.375045185697,0.00109621558353243,18.848589891905));
#27318=CARTESIAN_POINT('',(-2.37175,-1.78696459712734E-13,-1.84858989190501));
#27319=CARTESIAN_POINT('',(-2.34668236863849,0.343918483395781,19.62825));
#27320=CARTESIAN_POINT('Ctrl Pts',(-2.37315955426761,-0.00190203722427911,
18.651410108095));
#27321=CARTESIAN_POINT('Ctrl Pts',(-2.37434322924264,-0.13619766213342,
18.6604387279773));
#27322=CARTESIAN_POINT('Ctrl Pts',(-2.30301174794614,-1.05408217035119,
18.7222314607628));
#27323=CARTESIAN_POINT('Ctrl Pts',(-1.10630348664728,-2.57293846871273,
18.8367883064516));
#27324=CARTESIAN_POINT('Ctrl Pts',(1.55510431037697,-2.32895732784023,18.9950806451613));
#27325=CARTESIAN_POINT('Ctrl Pts',(2.799454735287,0.0339291128273711,19.153372983871));
#27326=CARTESIAN_POINT('Ctrl Pts',(1.49831225734699,2.36808646144409,19.3116653225806));
#27327=CARTESIAN_POINT('Ctrl Pts',(-1.17239605887113,2.54234418499522,19.4699576612903));
#27328=CARTESIAN_POINT('Ctrl Pts',(-2.23266420913401,1.1219063425307,19.5754858870968));
#27329=CARTESIAN_POINT('Ctrl Pts',(-2.34668236863853,0.34391848339548,19.62825));
#27330=CARTESIAN_POINT('',(-0.439445221993725,2.33068358199196,19.62825));
#27331=CARTESIAN_POINT('Origin',(0.,0.,19.62825));
#27332=CARTESIAN_POINT('Ctrl Pts',(-2.375045185697,0.0010962155835324,18.848589891905));
#27333=CARTESIAN_POINT('Ctrl Pts',(-2.3709070095079,-0.721840983553584,
18.8972862878202));
#27334=CARTESIAN_POINT('Ctrl Pts',(-1.63279314114456,-2.23594095261586,
18.9987802604312));
#27335=CARTESIAN_POINT('Ctrl Pts',(0.939403752255799,-2.63798173542721,
19.153071809738));
#27336=CARTESIAN_POINT('Ctrl Pts',(2.72681418428107,-0.648558891555657,
19.3114645398253));
#27337=CARTESIAN_POINT('Ctrl Pts',(2.02326260265721,1.93590572399224,19.4698572699127));
#27338=CARTESIAN_POINT('Ctrl Pts',(0.333728659905137,2.4764638032096,19.5754524233042));
#27339=CARTESIAN_POINT('Ctrl Pts',(-0.439445221994122,2.33068358199189,
19.62825));
#27340=CARTESIAN_POINT('Origin',(0.,0.,-1.84858989190501));
#27341=CARTESIAN_POINT('',(-2.36792071934755,-0.000146142683553414,17.651410108095));
#27342=CARTESIAN_POINT('',(-2.37168457540117,-0.00213991832454075,17.848589891905));
#27343=CARTESIAN_POINT('',(-2.37175,-1.78696459712734E-13,-1.84858989190501));
#27344=CARTESIAN_POINT('Ctrl Pts',(-2.36792071934755,-0.000146142683553653,
17.651410108095));
#27345=CARTESIAN_POINT('Ctrl Pts',(-2.36813419747129,-0.385740823797463,
17.6771873838913));
#27346=CARTESIAN_POINT('Ctrl Pts',(-2.09721693494845,-1.56033551046507,
17.7557287725908));
#27347=CARTESIAN_POINT('Ctrl Pts',(-0.252615203963521,-2.78904848883903,
17.8870342741935));
#27348=CARTESIAN_POINT('Ctrl Pts',(2.20107095869216,-1.73144044804223,18.0453266129032));
#27349=CARTESIAN_POINT('Ctrl Pts',(2.65111435612032,0.902257304582571,18.2036189516129));
#27350=CARTESIAN_POINT('Ctrl Pts',(0.687932462726838,2.71468339494958,18.3619112903226));
#27351=CARTESIAN_POINT('Ctrl Pts',(-1.75387752254126,2.09345318786399,18.51117500915));
#27352=CARTESIAN_POINT('Ctrl Pts',(-2.36742572016178,0.648638736727164,
18.6076746150741));
#27353=CARTESIAN_POINT('Ctrl Pts',(-2.37315955426761,-0.00190203722427911,
18.651410108095));
#27354=CARTESIAN_POINT('Ctrl Pts',(-2.37168457540117,-0.0021399183245409,
17.848589891905));
#27355=CARTESIAN_POINT('Ctrl Pts',(-2.37337117352649,-0.187581187441035,
17.8610365842831));
#27356=CARTESIAN_POINT('Ctrl Pts',(-2.26891520043147,-1.15776718319138,
17.9262808533569));
#27357=CARTESIAN_POINT('Ctrl Pts',(-0.936670484863442,-2.63980707365487,
18.0443226991266));
#27358=CARTESIAN_POINT('Ctrl Pts',(1.70458375322942,-2.22265690947637,18.2027154292139));
#27359=CARTESIAN_POINT('Ctrl Pts',(2.7924295091237,0.220067221674903,18.3611081593012));
#27360=CARTESIAN_POINT('Ctrl Pts',(1.33528471034559,2.46230981068379,18.5195008893886));
#27361=CARTESIAN_POINT('Ctrl Pts',(-1.33854848928615,2.46038562697746,18.6778936194759));
#27362=CARTESIAN_POINT('Ctrl Pts',(-2.34578650854474,0.906342840260155,
18.7875899536481));
#27363=CARTESIAN_POINT('Ctrl Pts',(-2.37539370037317,0.0619815458209781,
18.8444887111244));
#27364=CARTESIAN_POINT('Ctrl Pts',(-2.375045185697,0.0010962155835324,18.848589891905));
#27365=CARTESIAN_POINT('Origin',(0.,0.,-1.84858989190501));
#27366=CARTESIAN_POINT('',(-2.37266692485838,0.00204204400000237,16.651410108095));
#27367=CARTESIAN_POINT('',(-2.36805549047049,0.000622202524476756,16.848589891905));
#27368=CARTESIAN_POINT('',(-2.37175,-1.78696459712734E-13,-1.84858989190501));
#27369=CARTESIAN_POINT('Ctrl Pts',(-2.37266692485838,0.00204204400000234,
16.651410108095));
#27370=CARTESIAN_POINT('Ctrl Pts',(-2.36692591585228,-0.630870989238285,
16.6939360398053));
#27371=CARTESIAN_POINT('Ctrl Pts',(-1.78142766618931,-2.05845093397981,
16.7892260844188));
#27372=CARTESIAN_POINT('Ctrl Pts',(0.625834434246847,-2.72963661550809,
16.9372802419355));
#27373=CARTESIAN_POINT('Ctrl Pts',(2.62987209575649,-0.962474906809746,
17.0955725806452));
#27374=CARTESIAN_POINT('Ctrl Pts',(2.23996307264014,1.6808175336192,17.2538649193548));
#27375=CARTESIAN_POINT('Ctrl Pts',(-0.188960577202794,2.79407962162107,
17.4121572580645));
#27376=CARTESIAN_POINT('Ctrl Pts',(-2.07834764953227,1.59681365622726,17.5446723209779));
#27377=CARTESIAN_POINT('Ctrl Pts',(-2.36769722407223,0.403542010042759,
17.6244232709881));
#27378=CARTESIAN_POINT('Ctrl Pts',(-2.36792071934755,-0.000146142683553653,
17.651410108095));
#27379=CARTESIAN_POINT('Ctrl Pts',(-2.36805549047049,0.000622202524476895,
16.848589891905));
#27380=CARTESIAN_POINT('Ctrl Pts',(-2.36703221490523,-0.433037181511712,
16.8775844574417));
#27381=CARTESIAN_POINT('Ctrl Pts',(-2.04563496603972,-1.65777921929151,
16.9593765996742));
#27382=CARTESIAN_POINT('Ctrl Pts',(-0.0813612164248821,-2.79987490584551,
17.0939663186025));
#27383=CARTESIAN_POINT('Ctrl Pts',(2.3044540321531,-1.59229636617095,17.2523590486898));
#27384=CARTESIAN_POINT('Ctrl Pts',(2.59011097558326,1.0664174443023,17.4107517787772));
#27385=CARTESIAN_POINT('Ctrl Pts',(0.515273103550636,2.75325543193802,17.5691445088645));
#27386=CARTESIAN_POINT('Ctrl Pts',(-1.82920922018932,1.99553698989753,17.7150905465738));
#27387=CARTESIAN_POINT('Ctrl Pts',(-2.36621679940268,0.599041421309039,
17.8082390075873));
#27388=CARTESIAN_POINT('Ctrl Pts',(-2.37168457540117,-0.0021399183245409,
17.848589891905));
#27389=CARTESIAN_POINT('Origin',(0.,0.,-1.84858989190501));
#27390=CARTESIAN_POINT('',(-2.37421130889265,-0.00156313606789179,15.651410108095));
#27391=CARTESIAN_POINT('',(-2.37393561872375,0.00169440952702007,15.848589891905));
#27392=CARTESIAN_POINT('',(-2.37175,-1.78696459712734E-13,-1.84858989190501));
#27393=CARTESIAN_POINT('Ctrl Pts',(-2.37421130889265,-0.00156313606789185,
15.651410108095));
#27394=CARTESIAN_POINT('Ctrl Pts',(-2.37494957137993,-0.0982948133878638,
15.657920582816));
#27395=CARTESIAN_POINT('Ctrl Pts',(-2.32575783841749,-0.97823113259622,
15.7171951704403));
#27396=CARTESIAN_POINT('Ctrl Pts',(-1.22691420480089,-2.5173927084595,15.8292338709677));
#27397=CARTESIAN_POINT('Ctrl Pts',(1.44241955782089,-2.40041878462448,15.9875262096774));
#27398=CARTESIAN_POINT('Ctrl Pts',(2.7987333404768,-0.0983678276200387,
16.1458185483871));
#27399=CARTESIAN_POINT('Ctrl Pts',(1.60738835637255,2.29322636168875,16.3041108870968));
#27400=CARTESIAN_POINT('Ctrl Pts',(-1.0471460247291,2.59731972402479,16.4624032258064));
#27401=CARTESIAN_POINT('Ctrl Pts',(-2.29140475539041,1.09058640184897,16.5781696328059));
#27402=CARTESIAN_POINT('Ctrl Pts',(-2.37404908129966,0.154416796370487,
16.641171926902));
#27403=CARTESIAN_POINT('Ctrl Pts',(-2.37266692485838,0.00204204400000234,
16.651410108095));
#27404=CARTESIAN_POINT('Ctrl Pts',(-2.37393561872375,0.00169440952702,15.848589891905));
#27405=CARTESIAN_POINT('Ctrl Pts',(-2.36845987569029,-0.675173904700622,
15.8941323306004));
#27406=CARTESIAN_POINT('Ctrl Pts',(-1.71112283332055,-2.14603323350396,
15.9924723459915));
#27407=CARTESIAN_POINT('Ctrl Pts',(0.781808691918871,-2.68973858755105,
16.1436099380784));
#27408=CARTESIAN_POINT('Ctrl Pts',(2.68190993738254,-0.808255851442284,
16.3020026681657));
#27409=CARTESIAN_POINT('Ctrl Pts',(2.137857975385,1.80982921402577,16.4603953982531));
#27410=CARTESIAN_POINT('Ctrl Pts',(-0.354526606378597,2.77853009386107,
16.6187881283404));
#27411=CARTESIAN_POINT('Ctrl Pts',(-2.1267152976418,1.50123071247663,16.7481862928911));
#27412=CARTESIAN_POINT('Ctrl Pts',(-2.36889554581355,0.356633715936655,
16.824786880746));
#27413=CARTESIAN_POINT('Ctrl Pts',(-2.36805549047049,0.000622202524476895,
16.848589891905));
#27414=CARTESIAN_POINT('Origin',(0.,0.,-1.84858989190501));
#27415=CARTESIAN_POINT('',(-2.36813406422853,-0.000741801265089943,14.651410108095));
#27416=CARTESIAN_POINT('',(-2.3730883931612,-0.00196401976579913,14.848589891905));
#27417=CARTESIAN_POINT('',(-2.37175,-1.78696459712734E-13,-1.84858989190501));
#27418=CARTESIAN_POINT('Ctrl Pts',(-2.36813406422853,-0.000741801265090151,
14.651410108095));
#27419=CARTESIAN_POINT('Ctrl Pts',(-2.36911556130725,-0.348590331114078,
14.67466923873));
#27420=CARTESIAN_POINT('Ctrl Pts',(-2.13467349016726,-1.48428584342291,
14.7506924822682));
#27421=CARTESIAN_POINT('Ctrl Pts',(-0.384661101133316,-2.77391787153297,
14.8794798387097));
#27422=CARTESIAN_POINT('Ctrl Pts',(2.11642951734883,-1.833933100982,15.0377721774193));
#27423=CARTESIAN_POINT('Ctrl Pts',(2.69095567587589,0.775462488971503,15.196064516129));
#27424=CARTESIAN_POINT('Ctrl Pts',(0.815932002060255,2.67896239018596,15.3543568548387));
#27425=CARTESIAN_POINT('Ctrl Pts',(-1.69415942334001,2.16583952768063,15.5061387188274));
#27426=CARTESIAN_POINT('Ctrl Pts',(-2.36896632639394,0.68566662754189,15.6051564699128));
#27427=CARTESIAN_POINT('Ctrl Pts',(-2.37421130889265,-0.00156313606789185,
15.651410108095));
#27428=CARTESIAN_POINT('Ctrl Pts',(-2.3730883931612,-0.00196401976579899,
14.848589891905));
#27429=CARTESIAN_POINT('Ctrl Pts',(-2.3743190266956,-0.140204213139865,
14.8578826270632));
#27430=CARTESIAN_POINT('Ctrl Pts',(-2.30051483718045,-1.06255693428419,
14.9199729389172));
#27431=CARTESIAN_POINT('Ctrl Pts',(-1.09187025049414,-2.57948402526614,
15.034860827467));
#27432=CARTESIAN_POINT('Ctrl Pts',(1.56952811621541,-2.32002154590554,15.1932535575544));
#27433=CARTESIAN_POINT('Ctrl Pts',(2.80054018729513,0.0537879083119886,
15.3516462876417));
#27434=CARTESIAN_POINT('Ctrl Pts',(1.47928558581743,2.37857786000547,15.510039017729));
#27435=CARTESIAN_POINT('Ctrl Pts',(-1.19011296325406,2.53565565848489,15.6684317478164));
#27436=CARTESIAN_POINT('Ctrl Pts',(-2.31923158661152,1.00114407889721,15.7812820392084));
#27437=CARTESIAN_POINT('Ctrl Pts',(-2.37480793194414,0.109522913413036,
15.8413347539046));
#27438=CARTESIAN_POINT('Ctrl Pts',(-2.37393561872375,0.00169440952702,15.848589891905));
#27439=CARTESIAN_POINT('Origin',(0.,0.,-1.84858989190501));
#27440=CARTESIAN_POINT('',(-2.3715418496797,0.00213501335906034,13.651410108095));
#27441=CARTESIAN_POINT('',(-2.3679091445694,-0.000135598010815169,13.848589891905));
#27442=CARTESIAN_POINT('',(-2.37175,-1.78696459712734E-13,-1.84858989190501));
#27443=CARTESIAN_POINT('Ctrl Pts',(-2.3715418496797,0.00213501335906002,
13.651410108095));
#27444=CARTESIAN_POINT('Ctrl Pts',(-2.36615833382539,-0.594025841412108,
13.691417894644));
#27445=CARTESIAN_POINT('Ctrl Pts',(-1.83673527245257,-1.98495272027885,
13.7841897940962));
#27446=CARTESIAN_POINT('Ctrl Pts',(0.495613593829615,-2.7562568251976,13.9297258064516));
#27447=CARTESIAN_POINT('Ctrl Pts',(2.58124229901106,-1.08617342751133,14.0880181451613));
#27448=CARTESIAN_POINT('Ctrl Pts',(2.31719215337611,1.57264269469624,14.246310483871));
#27449=CARTESIAN_POINT('Ctrl Pts',(-0.0561746566308962,2.79989802113906,
14.4046028225806));
#27450=CARTESIAN_POINT('Ctrl Pts',(-2.03718260390642,1.67260737626565,14.5396360306553));
#27451=CARTESIAN_POINT('Ctrl Pts',(-2.36688900247802,0.440515650110908,
14.6219051258268));
#27452=CARTESIAN_POINT('Ctrl Pts',(-2.36813406422853,-0.000741801265090151,
14.651410108095));
#27453=CARTESIAN_POINT('Ctrl Pts',(-2.3679091445694,-0.000135598010815204,
13.848589891905));
#27454=CARTESIAN_POINT('Ctrl Pts',(-2.36810720184093,-0.386682243712472,
13.8744305002219));
#27455=CARTESIAN_POINT('Ctrl Pts',(-2.09616001129468,-1.5627590796402,13.9530686852345));
#27456=CARTESIAN_POINT('Ctrl Pts',(-0.247574124043378,-2.79009418007158,
14.084504446943));
#27457=CARTESIAN_POINT('Ctrl Pts',(2.20577578767506,-1.72640425598558,14.2428971770303));
#27458=CARTESIAN_POINT('Ctrl Pts',(2.64889636694473,0.910640718254001,14.4012899071176));
#27459=CARTESIAN_POINT('Ctrl Pts',(0.677950564144521,2.71777510348644,14.559682637205));
#27460=CARTESIAN_POINT('Ctrl Pts',(-1.75896225721554,2.08736146800612,14.7087826321341));
#27461=CARTESIAN_POINT('Ctrl Pts',(-2.36732706283238,0.645220862237953,
14.8050850503675));
#27462=CARTESIAN_POINT('Ctrl Pts',(-2.3730883931612,-0.00196401976579899,
14.848589891905));
#27463=CARTESIAN_POINT('Origin',(0.,0.,-1.84858989190501));
#27464=CARTESIAN_POINT('',(-2.37501984479867,-0.00103851368575368,12.651410108095));
#27465=CARTESIAN_POINT('',(-2.37259649009551,0.00206077343817647,12.848589891905));
#27466=CARTESIAN_POINT('',(-2.37175,-1.78696459712734E-13,-1.84858989190501));
#27467=CARTESIAN_POINT('Ctrl Pts',(-2.37501984479867,-0.00103851368575395,
12.651410108095));
#27468=CARTESIAN_POINT('Ctrl Pts',(-2.37534614220328,-0.0603027810327914,
12.6554024376547));
#27469=CARTESIAN_POINT('Ctrl Pts',(-2.3465255250126,-0.902503139782818,
12.7121588801177));
#27470=CARTESIAN_POINT('Ctrl Pts',(-1.3449778303753,-2.45634263828104,12.8216794354839));
#27471=CARTESIAN_POINT('Ctrl Pts',(1.3268996674641,-2.46615526545311,12.9799717741935));
#27472=CARTESIAN_POINT('Ctrl Pts',(2.79091377061401,-0.231051608597259,
13.1382641129033));
#27473=CARTESIAN_POINT('Ctrl Pts',(1.71438719543081,2.21437599900773,13.2965564516129));
#27474=CARTESIAN_POINT('Ctrl Pts',(-0.922728766019108,2.64407945137796,
13.4548487903226));
#27475=CARTESIAN_POINT('Ctrl Pts',(-2.26566734580998,1.16662759494473,13.5731333424833));
#27476=CARTESIAN_POINT('Ctrl Pts',(-2.37325836266616,0.192218571562817,
13.6386537817407));
#27477=CARTESIAN_POINT('Ctrl Pts',(-2.3715418496797,0.00213501335906002,
13.651410108095));
#27478=CARTESIAN_POINT('Ctrl Pts',(-2.37259649009551,0.00206077343817663,
12.848589891905));
#27479=CARTESIAN_POINT('Ctrl Pts',(-2.36684863781259,-0.628854604795339,
12.8909783733805));
#27480=CARTESIAN_POINT('Ctrl Pts',(-1.7843511132665,-2.05499140547376,12.9861644315518));
#27481=CARTESIAN_POINT('Ctrl Pts',(0.620614844457064,-2.73143839311951,
13.1341480664189));
#27482=CARTESIAN_POINT('Ctrl Pts',(2.62914881900703,-0.966175433387754,
13.2925407965062));
#27483=CARTESIAN_POINT('Ctrl Pts',(2.24161329961403,1.67960956640559,13.4509335265936));
#27484=CARTESIAN_POINT('Ctrl Pts',(-0.18881199672574,2.79468576238185,13.6093262566809));
#27485=CARTESIAN_POINT('Ctrl Pts',(-2.0787303718274,1.59642731960111,13.7418783784514));
#27486=CARTESIAN_POINT('Ctrl Pts',(-2.36770253087283,0.403110547644307,
13.8216329235261));
#27487=CARTESIAN_POINT('Ctrl Pts',(-2.3679091445694,-0.000135598010815204,
13.848589891905));
#27488=CARTESIAN_POINT('Origin',(0.,0.,-1.84858989190501));
#27489=CARTESIAN_POINT('',(-2.36862197310131,-0.00127836189895874,11.651410108095));
#27490=CARTESIAN_POINT('',(-2.37435526891825,-0.00149902739337487,11.848589891905));
#27491=CARTESIAN_POINT('',(-2.37175,-1.78696459712734E-13,-1.84858989190501));
#27492=CARTESIAN_POINT('Ctrl Pts',(-2.36862197310131,-0.00127836189895824,
11.651410108095));
#27493=CARTESIAN_POINT('Ctrl Pts',(-2.37014878532502,-0.31130720317775,
11.6721510935687));
#27494=CARTESIAN_POINT('Ctrl Pts',(-2.16971320797384,-1.40813889625016,
11.7456561919456));
#27495=CARTESIAN_POINT('Ctrl Pts',(-0.515844982015253,-2.75254218412146,
11.8719254032258));
#27496=CARTESIAN_POINT('Ctrl Pts',(2.02702915825758,-1.93228810284904,12.0302177419355));
#27497=CARTESIAN_POINT('Ctrl Pts',(2.72471908433383,0.646908364689661,12.1885100806452));
#27498=CARTESIAN_POINT('Ctrl Pts',(0.942124687882267,2.63723066744667,12.3468024193548));
#27499=CARTESIAN_POINT('Ctrl Pts',(-1.6314871656873,2.2372573077083,12.5011024285048));
#27500=CARTESIAN_POINT('Ctrl Pts',(-2.37103367429718,0.72295582691495,12.6026383247515));
#27501=CARTESIAN_POINT('Ctrl Pts',(-2.37501984479867,-0.00103851368575395,
12.651410108095));
#27502=CARTESIAN_POINT('Ctrl Pts',(-2.37435526891825,-0.00149902739337513,
11.848589891905));
#27503=CARTESIAN_POINT('Ctrl Pts',(-2.3750294186508,-0.09269358979894,11.8547286698434));
#27504=CARTESIAN_POINT('Ctrl Pts',(-2.32893572485017,-0.967534360360412,
11.9136650244775));
#27505=CARTESIAN_POINT('Ctrl Pts',(-1.24320306842743,-2.51005271084502,
12.0253989558075));
#27506=CARTESIAN_POINT('Ctrl Pts',(1.42890961951376,-2.40917740729671,12.1837916858948));
#27507=CARTESIAN_POINT('Ctrl Pts',(2.79878839655315,-0.112703113920128,
12.3421844159822));
#27508=CARTESIAN_POINT('Ctrl Pts',(1.61799699147824,2.28648293589416,12.5005771460695));
#27509=CARTESIAN_POINT('Ctrl Pts',(-1.03735272104025,2.60188735588576,12.6589698761568));
#27510=CARTESIAN_POINT('Ctrl Pts',(-2.28969978642726,1.09623807519608,12.7749741247687));
#27511=CARTESIAN_POINT('Ctrl Pts',(-2.37400795707056,0.156991028530352,
12.8381807966847));
#27512=CARTESIAN_POINT('Ctrl Pts',(-2.37259649009551,0.00206077343817663,
12.848589891905));
#27513=CARTESIAN_POINT('Origin',(0.,0.,-1.84858989190501));
#27514=CARTESIAN_POINT('',(-2.3704600388318,0.00204051513951079,10.651410108095));
#27515=CARTESIAN_POINT('',(-2.36821409753223,-0.000876700279052733,10.848589891905));
#27516=CARTESIAN_POINT('',(-2.37175,-1.78696459712734E-13,-1.84858989190501));
#27517=CARTESIAN_POINT('Ctrl Pts',(-2.3704600388318,0.00204051513951101,
10.651410108095));
#27518=CARTESIAN_POINT('Ctrl Pts',(-2.36581720590312,-0.557246380947459,
10.6888997494827));
#27519=CARTESIAN_POINT('Ctrl Pts',(-1.88917186759772,-1.91081278379687,
10.7791535037736));
#27520=CARTESIAN_POINT('Ctrl Pts',(0.364276246834986,-2.77666838798409,
10.9221713709677));
#27521=CARTESIAN_POINT('Ctrl Pts',(2.52679819661009,-1.20742510924963,11.0804637096774));
#27522=CARTESIAN_POINT('Ctrl Pts',(2.38920121328945,1.46092507790601,11.2387560483871));
#27523=CARTESIAN_POINT('Ctrl Pts',(0.0767384440762257,2.79940988996594,
11.3970483870968));
#27524=CARTESIAN_POINT('Ctrl Pts',(-1.99342445870054,1.74813839309205,11.5345997403327));
#27525=CARTESIAN_POINT('Ctrl Pts',(-2.36626464526543,0.477391906863246,
11.6193869806655));
#27526=CARTESIAN_POINT('Ctrl Pts',(-2.36862197310131,-0.00127836189895824,
11.651410108095));
#27527=CARTESIAN_POINT('Ctrl Pts',(-2.36821409753223,-0.000876700279052144,
10.848589891905));
#27528=CARTESIAN_POINT('Ctrl Pts',(-2.36934663768308,-0.34013449210219,
10.871276543002));
#27529=CARTESIAN_POINT('Ctrl Pts',(-2.14277840224568,-1.46748838032652,
10.9467607707948));
#27530=CARTESIAN_POINT('Ctrl Pts',(-0.412912081686591,-2.77045521410563,
11.0750425752834));
#27531=CARTESIAN_POINT('Ctrl Pts',(2.09930342438264,-1.85441193183801,11.2334353053708));
#27532=CARTESIAN_POINT('Ctrl Pts',(2.69832297238025,0.751645938785551,11.3918280354581));
#27533=CARTESIAN_POINT('Ctrl Pts',(0.838231300737091,2.67269279323914,11.5502207655454));
#27534=CARTESIAN_POINT('Ctrl Pts',(-1.68408275985356,2.17793475487982,11.7024747176944));
#27535=CARTESIAN_POINT('Ctrl Pts',(-2.3692312821868,0.691640352752269,11.8019310931476));
#27536=CARTESIAN_POINT('Ctrl Pts',(-2.37435526891825,-0.00149902739337513,
11.848589891905));
#27537=CARTESIAN_POINT('Origin',(0.,0.,-1.84858989190501));
#27538=CARTESIAN_POINT('',(-2.37550470632433,-0.000400580813136427,9.65141010809499));
#27539=CARTESIAN_POINT('',(-2.371188773444,0.00213200020334231,9.84858989190502));
#27540=CARTESIAN_POINT('',(-2.37175,-1.78696459712734E-13,-1.84858989190501));
#27541=CARTESIAN_POINT('Ctrl Pts',(-2.37550470632433,-0.000400580813136008,
9.65141010809499));
#27542=CARTESIAN_POINT('Ctrl Pts',(-2.3755561297693,-0.022272253864447,
9.65288429249344));
#27543=CARTESIAN_POINT('Ctrl Pts',(-2.36539776597002,-0.826927449365476,
9.70712258979511));
#27544=CARTESIAN_POINT('Ctrl Pts',(-1.46001177080394,-2.38975943348956,
9.81412499999998));
#27545=CARTESIAN_POINT('Ctrl Pts',(1.20839081375242,-2.52633651006299,9.97241733870969));
#27546=CARTESIAN_POINT('Ctrl Pts',(2.77680741881119,-0.363214922151578,
10.1307096774193));
#27547=CARTESIAN_POINT('Ctrl Pts',(1.81752421541791,2.13053754888476,10.2890020161291));
#27548=CARTESIAN_POINT('Ctrl Pts',(-0.796232964112916,2.68488316090261,
10.4472943548387));
#27549=CARTESIAN_POINT('Ctrl Pts',(-2.23781112805667,1.24275389167182,10.5680970521607));
#27550=CARTESIAN_POINT('Ctrl Pts',(-2.37235167654013,0.229911773627901,
10.6361356365795));
#27551=CARTESIAN_POINT('Ctrl Pts',(-2.3704600388318,0.00204051513951101,
10.651410108095));
#27552=CARTESIAN_POINT('Ctrl Pts',(-2.371188773444,0.00213200020334229,
9.84858989190502));
#27553=CARTESIAN_POINT('Ctrl Pts',(-2.36599120092886,-0.582728163373476,
9.88782441616068));
#27554=CARTESIAN_POINT('Ctrl Pts',(-1.85298786413136,-1.96277949353793,
9.97985651711213));
#27555=CARTESIAN_POINT('Ctrl Pts',(0.457228155062243,-2.76348708967243,
10.1246861947593));
#27556=CARTESIAN_POINT('Ctrl Pts',(2.56709800604834,-1.12068118031423,10.2830789248467));
#27557=CARTESIAN_POINT('Ctrl Pts',(2.33744824681434,1.54345527114731,10.441471654934));
#27558=CARTESIAN_POINT('Ctrl Pts',(-0.0224302759543461,2.80096686222604,
10.5998643850214));
#27559=CARTESIAN_POINT('Ctrl Pts',(-2.02678859651666,1.69132688976849,10.7355704640117));
#27560=CARTESIAN_POINT('Ctrl Pts',(-2.36671093022588,0.44940421975213,10.8184789663063));
#27561=CARTESIAN_POINT('Ctrl Pts',(-2.36821409753223,-0.000876700279052144,
10.848589891905));
#27562=CARTESIAN_POINT('Origin',(0.,0.,-1.84858989190501));
#27563=CARTESIAN_POINT('',(-2.36935474920583,-0.00171244552815533,8.65141010809499));
#27564=CARTESIAN_POINT('',(-2.37526986480305,-0.00079584354989698,8.84858989190502));
#27565=CARTESIAN_POINT('',(-2.37175,-1.78696459712734E-13,-1.84858989190501));
#27566=CARTESIAN_POINT('Ctrl Pts',(-2.36935474920583,-0.00171244552815496,
8.65141010809499));
#27567=CARTESIAN_POINT('Ctrl Pts',(-2.37118720028221,-0.27388934122613,
8.66963294840741));
#27568=CARTESIAN_POINT('Ctrl Pts',(-2.2024097115759,-1.33194990712133,8.74061990162306));
#27569=CARTESIAN_POINT('Ctrl Pts',(-0.645866875421753,-2.72496614659181,
8.86437096774193));
#27570=CARTESIAN_POINT('Ctrl Pts',(1.93306273270264,-2.02629045111372,9.02266330645161));
#27571=CARTESIAN_POINT('Ctrl Pts',(2.75234481681179,0.516897020892659,9.18095564516129));
#27572=CARTESIAN_POINT('Ctrl Pts',(1.06619515253284,2.58955834411081,9.33924798387097));
#27573=CARTESIAN_POINT('Ctrl Pts',(-1.56575926891701,2.3076211823316,9.49606613818219));
#27574=CARTESIAN_POINT('Ctrl Pts',(-2.37371557816729,0.760560224541533,
9.60012017959021));
#27575=CARTESIAN_POINT('Ctrl Pts',(-2.37550470632433,-0.000400580813136008,
9.65141010809499));
#27576=CARTESIAN_POINT('Ctrl Pts',(-2.37526986480305,-0.000795843549896919,
8.84858989190502));
#27577=CARTESIAN_POINT('Ctrl Pts',(-2.37546378554503,-0.0450917311895661,
8.85157471262355));
#27578=CARTESIAN_POINT('Ctrl Pts',(-2.35430174920285,-0.872735026693859,
8.90735711003785));
#27579=CARTESIAN_POINT('Ctrl Pts',(-1.39014322226223,-2.43175251663614,
9.01593708414793));
#27580=CARTESIAN_POINT('Ctrl Pts',(1.2832422936176,-2.48982081613093,9.17432981423527));
#27581=CARTESIAN_POINT('Ctrl Pts',(2.78714752338885,-0.278795917178183,
9.33272254432263));
#27582=CARTESIAN_POINT('Ctrl Pts',(1.75099145741626,2.18630908076216,9.49111527440996));
#27583=CARTESIAN_POINT('Ctrl Pts',(-0.880927155331511,2.6589256904937,9.64950800449731));
#27584=CARTESIAN_POINT('Ctrl Pts',(-2.25694217263034,1.19150479465494,9.76866621032899));
#27585=CARTESIAN_POINT('Ctrl Pts',(-2.37298553152687,0.2043133499004,9.83502683946489));
#27586=CARTESIAN_POINT('Ctrl Pts',(-2.371188773444,0.00213200020334229,
9.84858989190502));
#27587=CARTESIAN_POINT('Origin',(0.,0.,-1.84858989190501));
#27588=CARTESIAN_POINT('',(-2.36950128627827,0.0017735229177115,7.65141010809498));
#27589=CARTESIAN_POINT('',(-2.36894127455122,-0.00150910447186903,7.84858989190502));
#27590=CARTESIAN_POINT('',(-2.37175,-1.78696459712734E-13,-1.84858989190501));
#27591=CARTESIAN_POINT('Ctrl Pts',(-2.36950128627827,0.00177352291771137,
7.65141010809498));
#27592=CARTESIAN_POINT('Ctrl Pts',(-2.36584417946481,-0.520480430603125,
7.68638160432139));
#27593=CARTESIAN_POINT('Ctrl Pts',(-1.93879965313242,-1.83613375809405,
7.77411721345102));
#27594=CARTESIAN_POINT('Ctrl Pts',(0.23211833466387,-2.79082525421268,7.91461693548387));
#27595=CARTESIAN_POINT('Ctrl Pts',(2.4666622528453,-1.32595695677747,8.07290927419355));
#27596=CARTESIAN_POINT('Ctrl Pts',(2.45582838148514,1.34591659530986,8.23120161290321));
#27597=CARTESIAN_POINT('Ctrl Pts',(0.209478684497901,2.79261583494391,8.38949395161291));
#27598=CARTESIAN_POINT('Ctrl Pts',(-1.94700227603872,1.8233279802371,8.52956345001015));
#27599=CARTESIAN_POINT('Ctrl Pts',(-2.36588135038034,0.51419704970092,8.61686883550418));
#27600=CARTESIAN_POINT('Ctrl Pts',(-2.36935474920583,-0.00171244552815496,
8.65141010809499));
#27601=CARTESIAN_POINT('Ctrl Pts',(-2.36894127455122,-0.0015091044718692,
7.84858989190502));
#27602=CARTESIAN_POINT('Ctrl Pts',(-2.37065112362024,-0.29337775612239,
7.86812258578219));
#27603=CARTESIAN_POINT('Ctrl Pts',(-2.18563237695357,-1.37208652926944,
7.94045285635514));
#27604=CARTESIAN_POINT('Ctrl Pts',(-0.576791078891976,-2.74102727674834,
8.06558070362385));
#27605=CARTESIAN_POINT('Ctrl Pts',(1.9854134998704,-1.97586733236324,8.22397343371122));
#27606=CARTESIAN_POINT('Ctrl Pts',(2.73821547444757,0.589995335628766,8.38236616379854));
#27607=CARTESIAN_POINT('Ctrl Pts',(0.995550277773485,2.61816693986326,8.54075889388591));
#27608=CARTESIAN_POINT('Ctrl Pts',(-1.60447071736692,2.26702158872423,8.69616680325471));
#27609=CARTESIAN_POINT('Ctrl Pts',(-2.37203358111632,0.738444616722348,
8.79877713592776));
#27610=CARTESIAN_POINT('Ctrl Pts',(-2.37526986480305,-0.000795843549896919,
8.84858989190502));
#27611=CARTESIAN_POINT('Origin',(0.,0.,-1.84858989190501));
#27612=CARTESIAN_POINT('',(-2.37554636470555,0.000284697057196372,6.65141010809498));
#27613=CARTESIAN_POINT('',(-2.36989007687564,0.00191473874719905,6.84858989190502));
#27614=CARTESIAN_POINT('',(-2.37175,-1.78696459712734E-13,-1.84858989190501));
#27615=CARTESIAN_POINT('Ctrl Pts',(-2.37554636470555,0.000284697057196357,
6.65141010809498));
#27616=CARTESIAN_POINT('Ctrl Pts',(-2.37423866256909,-0.767022922389114,
6.70313026023536));
#27617=CARTESIAN_POINT('Ctrl Pts',(-1.55422096328597,-2.31952782580344,
6.80761452527896));
#27618=CARTESIAN_POINT('Ctrl Pts',(1.087159950493,-2.58082695330052,6.96486290322581));
#27619=CARTESIAN_POINT('Ctrl Pts',(2.75644605727123,-0.494560061258782,
7.12315524193547));
#27620=CARTESIAN_POINT('Ctrl Pts',(1.91656709780378,2.04189987033018,7.28144758064516));
#27621=CARTESIAN_POINT('Ctrl Pts',(-0.667943575474826,2.7196389283911,7.43973991935484));
#27622=CARTESIAN_POINT('Ctrl Pts',(-2.20776674506755,1.31893238938929,7.56306076183811));
#27623=CARTESIAN_POINT('Ctrl Pts',(-2.37136193013682,0.267483183802526,
7.63361749141816));
#27624=CARTESIAN_POINT('Ctrl Pts',(-2.36950128627827,0.00177352291771137,
7.65141010809498));
#27625=CARTESIAN_POINT('Ctrl Pts',(-2.36989007687564,0.00191473874719891,
6.84858989190502));
#27626=CARTESIAN_POINT('Ctrl Pts',(-2.36577478375809,-0.53667818893527,
6.88467045894083));
#27627=CARTESIAN_POINT('Ctrl Pts',(-1.91714943575642,-1.86961076393625,
6.97354860267242));
#27628=CARTESIAN_POINT('Ctrl Pts',(0.292225921295444,-2.78577143561543,
7.11522432309981));
#27629=CARTESIAN_POINT('Ctrl Pts',(2.49597675267592,-1.27122717508287,7.27361705318714));
#27630=CARTESIAN_POINT('Ctrl Pts',(2.42502418520658,1.40184741742138,7.43200978327449));
#27631=CARTESIAN_POINT('Ctrl Pts',(0.144030698698804,2.79735118252968,7.59040251336184));
#27632=CARTESIAN_POINT('Ctrl Pts',(-1.9707500505419,1.78578599745412,7.729262549572));
#27633=CARTESIAN_POINT('Ctrl Pts',(-2.36602933985975,0.495553745979654,
7.8153250090864));
#27634=CARTESIAN_POINT('Ctrl Pts',(-2.36894127455122,-0.0015091044718692,
7.84858989190502));
#27635=CARTESIAN_POINT('Origin',(0.,0.,-1.84858989190501));
#27636=CARTESIAN_POINT('',(-2.37028552428411,-0.00200651108796764,5.65141010809498));
#27637=CARTESIAN_POINT('',(-2.3755997202681,4.64207010002296E-5,5.84858989190501));
#27638=CARTESIAN_POINT('',(-2.37175,-1.78696459712734E-13,-1.84858989190501));
#27639=CARTESIAN_POINT('Ctrl Pts',(-2.37028552428411,-0.00200651108796798,
5.65141010809498));
#27640=CARTESIAN_POINT('Ctrl Pts',(-2.37218747443614,-0.236339757801373,
5.66711480324611));
#27641=CARTESIAN_POINT('Ctrl Pts',(-2.23283499221027,-1.25576625306762,
5.73558361130047));
#27642=CARTESIAN_POINT('Ctrl Pts',(-0.774433895304387,-2.6912518764775,
5.85681653225807));
#27643=CARTESIAN_POINT('Ctrl Pts',(1.83474190859146,-2.11572839695838,6.01510887096773));
#27644=CARTESIAN_POINT('Ctrl Pts',(2.77377064377508,0.385721319828002,6.17340120967742));
#27645=CARTESIAN_POINT('Ctrl Pts',(1.18786391621721,2.53605280650616,6.3316935483871));
#27646=CARTESIAN_POINT('Ctrl Pts',(-1.47934336288373,2.37784098196877,6.48998588709676));
#27647=CARTESIAN_POINT('Ctrl Pts',(-2.36843670110272,0.814031196077336,
6.59655807366607));
#27648=CARTESIAN_POINT('Ctrl Pts',(-2.37557276040749,0.0157726454599615,
6.65036614733214));
#27649=CARTESIAN_POINT('Ctrl Pts',(-2.37554636470555,0.000284697057196357,
6.65141010809498));
#27650=CARTESIAN_POINT('Ctrl Pts',(-2.37559927670797,4.64153524631309E-5,
5.84858989190501));
#27651=CARTESIAN_POINT('Ctrl Pts',(-2.37537320011125,-0.780689829870116,
5.90121833209947));
#27652=CARTESIAN_POINT('Ctrl Pts',(-1.52932552826367,-2.34509161690763,
6.00664434898972));
#27653=CARTESIAN_POINT('Ctrl Pts',(1.13304083122442,-2.56166683144901,6.16486794257572));
#27654=CARTESIAN_POINT('Ctrl Pts',(2.76565869916243,-0.443903638546721,
6.32326067266308));
#27655=CARTESIAN_POINT('Ctrl Pts',(1.87779906814186,2.07841024349223,6.48165340275042));
#27656=CARTESIAN_POINT('Ctrl Pts',(-0.721388970917745,2.70656912588725,
6.64004613283776));
#27657=CARTESIAN_POINT('Ctrl Pts',(-2.22082549341992,1.28688950604137,6.7623582958893));
#27658=CARTESIAN_POINT('Ctrl Pts',(-2.37179679288516,0.251458022419059,
6.83187288224505));
#27659=CARTESIAN_POINT('Ctrl Pts',(-2.36989007687564,0.00191473874719891,
6.84858989190502));
#27660=CARTESIAN_POINT('Origin',(0.,0.,-1.84858989190501));
#27661=CARTESIAN_POINT('',(-2.36873091192997,0.00136091434597342,4.65141010809498));
#27662=CARTESIAN_POINT('',(-2.37001948420046,-0.00195088435344298,4.84858989190502));
#27663=CARTESIAN_POINT('',(-2.37175,-1.78696459712734E-13,-1.84858989190501));
#27664=CARTESIAN_POINT('Ctrl Pts',(-2.36873091192997,0.00136091434597342,
4.65141010809498));
#27665=CARTESIAN_POINT('Ctrl Pts',(-2.36618048682385,-0.483684235607871,
4.6838634591601));
#27666=CARTESIAN_POINT('Ctrl Pts',(-1.98568385961058,-1.76101097954328,
4.76908092312844));
#27667=CARTESIAN_POINT('Ctrl Pts',(0.099437554957728,-2.79869553427603,
4.9070625));
#27668=CARTESIAN_POINT('Ctrl Pts',(2.40096992936847,-1.44150196638533,5.06535483870968));
#27669=CARTESIAN_POINT('Ctrl Pts',(2.51692357424149,1.22787631390688,5.22364717741935));
#27670=CARTESIAN_POINT('Ctrl Pts',(0.341747055246021,2.77953116030023,5.38193951612902));
#27671=CARTESIAN_POINT('Ctrl Pts',(-1.8978479262878,1.89808937168119,5.52452715968758));
#27672=CARTESIAN_POINT('Ctrl Pts',(-2.36579736551696,0.550965297634364,
5.61435069034289));
#27673=CARTESIAN_POINT('Ctrl Pts',(-2.37028552428411,-0.00200651108796798,
5.65141010809498));
#27674=CARTESIAN_POINT('Ctrl Pts',(-2.37001948420046,-0.00195088435344316,
4.84858989190502));
#27675=CARTESIAN_POINT('Ctrl Pts',(-2.37193026582578,-0.24641085904258,
4.86496862856234));
#27676=CARTESIAN_POINT('Ctrl Pts',(-2.22486407851201,-1.27665550423204,
4.93414494191544));
#27677=CARTESIAN_POINT('Ctrl Pts',(-0.738632074782922,-2.7019143470289,
5.05611883196433));
#27678=CARTESIAN_POINT('Ctrl Pts',(1.86450842642192,-2.09034131384488,5.21451156205166));
#27679=CARTESIAN_POINT('Ctrl Pts',(2.76843291921558,0.426260075974678,5.37290429213902));
#27680=CARTESIAN_POINT('Ctrl Pts',(1.14935163317956,2.55439020196149,5.53129702222635));
#27681=CARTESIAN_POINT('Ctrl Pts',(-1.51718895457673,2.35458194945041,5.68968975231371));
#27682=CARTESIAN_POINT('Ctrl Pts',(-2.37446221325061,0.788309337875694,
5.79545404220658));
#27683=CARTESIAN_POINT('Ctrl Pts',(-2.37560000326959,0.00255553392953162,
5.84842075540369));
#27684=CARTESIAN_POINT('Ctrl Pts',(-2.37559927670797,4.64153524631309E-5,
5.84858989190501));
#27685=CARTESIAN_POINT('Origin',(0.,0.,-1.84858989190501));
#27686=CARTESIAN_POINT('',(-2.37512893756715,0.000936004496838188,3.65141010809498));
#27687=CARTESIAN_POINT('',(-2.36884487406159,0.0014490806830475,3.84858989190502));
#27688=CARTESIAN_POINT('',(-2.37175,-1.78696459712734E-13,-1.84858989190501));
#27689=CARTESIAN_POINT('Ctrl Pts',(-2.37512893756715,0.000936004496838207,
3.65141010809498));
#27690=CARTESIAN_POINT('Ctrl Pts',(-2.37144701194991,-0.729355776449451,
3.70061211507407));
#27691=CARTESIAN_POINT('Ctrl Pts',(-1.62047524979812,-2.24935719258021,
3.80257823495639));
#27692=CARTESIAN_POINT('Ctrl Pts',(0.963480161046465,-2.62950385116291,
3.95730846774193));
#27693=CARTESIAN_POINT('Ctrl Pts',(2.72987555186367,-0.62479115878066,4.11560080645161));
#27694=CARTESIAN_POINT('Ctrl Pts',(2.01129273950979,1.94866262755053,4.27389314516129));
#27695=CARTESIAN_POINT('Ctrl Pts',(-0.538149583533225,2.74826846342811,
4.43218548387097));
#27696=CARTESIAN_POINT('Ctrl Pts',(-2.17546335777147,1.39512363286222,4.55802447151553));
#27697=CARTESIAN_POINT('Ctrl Pts',(-2.37032708228576,0.304923911636404,
4.63109934625687));
#27698=CARTESIAN_POINT('Ctrl Pts',(-2.36873091192997,0.00136091434597342,
4.65141010809498));
#27699=CARTESIAN_POINT('Ctrl Pts',(-2.36884487406159,0.0014490806830475,
3.84858989190502));
#27700=CARTESIAN_POINT('Ctrl Pts',(-2.36608421378806,-0.490609372151221,
3.88151650172098));
#27701=CARTESIAN_POINT('Ctrl Pts',(-1.97696067069986,-1.77568073879797,
3.96724068823273));
#27702=CARTESIAN_POINT('Ctrl Pts',(0.126191152782097,-2.79821269277661,
4.10576245144026));
#27703=CARTESIAN_POINT('Ctrl Pts',(2.41603635476259,-1.41728148685534,4.26415518152759));
#27704=CARTESIAN_POINT('Ctrl Pts',(2.50403167886292,1.25528635446798,4.42254791161495));
#27705=CARTESIAN_POINT('Ctrl Pts',(0.309982763347203,2.78385149874581,4.58094064170228));
#27706=CARTESIAN_POINT('Ctrl Pts',(-1.91047842319259,1.87964319012959,4.72295463513232));
#27707=CARTESIAN_POINT('Ctrl Pts',(-2.36577077736693,0.541616601972229,
4.81217105186656));
#27708=CARTESIAN_POINT('Ctrl Pts',(-2.37001948420046,-0.00195088435344316,
4.84858989190502));
#27709=CARTESIAN_POINT('Origin',(0.,0.,-1.84858989190501));
#27710=CARTESIAN_POINT('',(-2.37135157935354,-0.0021318991616305,2.65141010809498));
#27711=CARTESIAN_POINT('',(-2.37519554933426,0.000880106332527136,2.84858989190502));
#27712=CARTESIAN_POINT('',(-2.37175,-1.78696459712734E-13,-1.84858989190501));
#27713=CARTESIAN_POINT('Ctrl Pts',(-2.37135157935354,-0.00213189916163091,
2.65141010809498));
#27714=CARTESIAN_POINT('Ctrl Pts',(-2.37311082894275,-0.198666550155835,
2.66459665808482));
#27715=CARTESIAN_POINT('Ctrl Pts',(-2.26106011094342,-1.17962859930864,
2.7305473209779));
#27716=CARTESIAN_POINT('Ctrl Pts',(-0.901256421879981,-2.65147525836599,
2.84926209677419));
#27717=CARTESIAN_POINT('Ctrl Pts',(1.73228815673516,-2.20040050466946,3.00755443548387));
#27718=CARTESIAN_POINT('Ctrl Pts',(2.78894830461411,0.253676763035589,3.16584677419355));
#27719=CARTESIAN_POINT('Ctrl Pts',(1.30685690747379,2.47683457209687,3.32413911290322));
#27720=CARTESIAN_POINT('Ctrl Pts',(-1.36485315638996,2.44535486220292,3.4824314516129));
#27721=CARTESIAN_POINT('Ctrl Pts',(-2.34988246062014,0.889580033391542,
3.59152178334349));
#27722=CARTESIAN_POINT('Ctrl Pts',(-2.37539550004821,0.0538073574959181,
3.64784800217084));
#27723=CARTESIAN_POINT('Ctrl Pts',(-2.37512893756715,0.000936004496838207,
3.65141010809498));
#27724=CARTESIAN_POINT('Ctrl Pts',(-2.37519554933426,0.00088010633252705,
2.84858989190502));
#27725=CARTESIAN_POINT('Ctrl Pts',(-2.37168702189121,-0.733401409280994,
2.89806437487963));
#27726=CARTESIAN_POINT('Ctrl Pts',(-1.61323878014562,-2.25754538560165,
3.00033643455002));
#27727=CARTESIAN_POINT('Ctrl Pts',(0.978835944215164,-2.62446160086853,
3.15540607091619));
#27728=CARTESIAN_POINT('Ctrl Pts',(2.73439785209926,-0.607442893388946,
3.31379880100354));
#27729=CARTESIAN_POINT('Ctrl Pts',(1.99797176831316,1.9631676666159,3.47219153109088));
#27730=CARTESIAN_POINT('Ctrl Pts',(-0.559301870866465,2.7446493220368,3.63058426117822));
#27731=CARTESIAN_POINT('Ctrl Pts',(-2.18121205708018,1.38232176842859,3.7560503814496));
#27732=CARTESIAN_POINT('Ctrl Pts',(-2.37051091223462,0.29840273834331,3.8287189250252));
#27733=CARTESIAN_POINT('Ctrl Pts',(-2.36884487406159,0.0014490806830475,
3.84858989190502));
#27734=CARTESIAN_POINT('Origin',(0.,0.,-1.84858989190501));
#27735=CARTESIAN_POINT('',(-2.36819810156307,0.000841410002426573,1.65141010809498));
#27736=CARTESIAN_POINT('',(-2.37133740986255,-0.00213858212026324,1.84858989190502));
#27737=CARTESIAN_POINT('',(-2.37175,-1.78696459712734E-13,-1.84858989190501));
#27738=CARTESIAN_POINT('Ctrl Pts',(-2.36819810156307,0.000841410002426421,
1.65141010809498));
#27739=CARTESIAN_POINT('Ctrl Pts',(-2.36676749726595,-0.446820888278083,
1.6813453139988));
#27740=CARTESIAN_POINT('Ctrl Pts',(-2.02989303093846,-1.68553679022923,
1.76404463280585));
#27741=CARTESIAN_POINT('Ctrl Pts',(-0.0334666860564693,-2.80025859792997,
1.89950806451613));
#27742=CARTESIAN_POINT('Ctrl Pts',(2.32986892611582,-1.55380138209287,2.0578004032258));
#27743=CARTESIAN_POINT('Ctrl Pts',(2.57234931467855,1.10707092589757,2.21609274193548));
#27744=CARTESIAN_POINT('Ctrl Pts',(0.473245533627712,2.76018492369889,2.37438508064516));
#27745=CARTESIAN_POINT('Ctrl Pts',(-1.84589567906405,1.97232864399116,2.51949086936499));
#27746=CARTESIAN_POINT('Ctrl Pts',(-2.36607144077667,0.587739031473957,
2.6118325451816));
#27747=CARTESIAN_POINT('Ctrl Pts',(-2.37135157935354,-0.00213189916163091,
2.65141010809498));
#27748=CARTESIAN_POINT('Ctrl Pts',(-2.37133740986255,-0.00213858212026316,
1.84858989190502));
#27749=CARTESIAN_POINT('Ctrl Pts',(-2.37310428453163,-0.199245954569927,
1.86181467134249));
#27750=CARTESIAN_POINT('Ctrl Pts',(-2.26061413178437,-1.18128083118873,
1.92783702747574));
#27751=CARTESIAN_POINT('Ctrl Pts',(-0.897863084978552,-2.65325422541087,
2.04665696030478));
#27752=CARTESIAN_POINT('Ctrl Pts',(1.7370153276097,-2.19742960924133,2.20504969039212));
#27753=CARTESIAN_POINT('Ctrl Pts',(2.78886857766781,0.261018802222555,2.36344242047947));
#27754=CARTESIAN_POINT('Ctrl Pts',(1.29909191311228,2.48158786740548,2.52183515056681));
#27755=CARTESIAN_POINT('Ctrl Pts',(-1.37460948338166,2.44056701717432,2.68022788065416));
#27756=CARTESIAN_POINT('Ctrl Pts',(-2.35172378535123,0.882891152726273,
2.78914612776689));
#27757=CARTESIAN_POINT('Ctrl Pts',(-2.37543120951332,0.0502002032269103,
2.84526679818384));
#27758=CARTESIAN_POINT('Ctrl Pts',(-2.37519554933426,0.00088010633252705,
2.84858989190502));
#27759=CARTESIAN_POINT('Origin',(0.,0.,-1.84858989190501));
#27760=CARTESIAN_POINT('',(-2.37433784198147,0.00164420209662431,0.651410108094979));
#27761=CARTESIAN_POINT('',(-2.36815429608613,0.000817443606317692,0.848589891905017));
#27762=CARTESIAN_POINT('',(-2.37175,-1.78696459712734E-13,-1.84858989190501));
#27763=CARTESIAN_POINT('Ctrl Pts',(-2.37433784198147,0.00164420209662409,
0.651410108094979));
#27764=CARTESIAN_POINT('Ctrl Pts',(-2.36924246624065,-0.691823527182799,
0.698093969912781));
#27765=CARTESIAN_POINT('Ctrl Pts',(-1.6837126199259,-2.17836324814241,0.797541944633808));
#27766=CARTESIAN_POINT('Ctrl Pts',(0.837655777364047,-2.67211687161305,
0.949754032258061));
#27767=CARTESIAN_POINT('Ctrl Pts',(2.69714227944592,-0.753688528678065,
1.10804637096774));
#27768=CARTESIAN_POINT('Ctrl Pts',(2.10149481948277,1.85107442631988,1.26633870967742));
#27769=CARTESIAN_POINT('Ctrl Pts',(-0.407147056663944,2.77068707131458,
1.42463104838709));
#27770=CARTESIAN_POINT('Ctrl Pts',(-2.14082823127596,1.47128617579538,1.55298818119295));
#27771=CARTESIAN_POINT('Ctrl Pts',(-2.36928909564398,0.342233448775053,
1.62858120109558));
#27772=CARTESIAN_POINT('Ctrl Pts',(-2.36819810156307,0.000841410002426421,
1.65141010809498));
#27773=CARTESIAN_POINT('Ctrl Pts',(-2.36815429608612,0.000817443606317657,
0.848589891905016));
#27774=CARTESIAN_POINT('Ctrl Pts',(-2.36680126784445,-0.444438138072723,
0.878362544501135));
#27775=CARTESIAN_POINT('Ctrl Pts',(-2.03256363798364,-1.68119575265189,
0.960932773793035));
#27776=CARTESIAN_POINT('Ctrl Pts',(-0.0402824848387021,-2.80074754850057,
1.09630057978071));
#27777=CARTESIAN_POINT('Ctrl Pts',(2.32755559974952,-1.55833818967747,1.25469330986806));
#27778=CARTESIAN_POINT('Ctrl Pts',(2.57419348860935,1.10429523958194,1.4130860399554));
#27779=CARTESIAN_POINT('Ctrl Pts',(0.474838546093255,2.76051273114501,1.57147877004275));
#27780=CARTESIAN_POINT('Ctrl Pts',(-1.84584231488806,1.97272007570003,1.71664672069262));
#27781=CARTESIAN_POINT('Ctrl Pts',(-2.36605035207901,0.587670126973683,
1.80901709464671));
#27782=CARTESIAN_POINT('Ctrl Pts',(-2.37133740986255,-0.00213858212026316,
1.84858989190502));
#27783=CARTESIAN_POINT('Origin',(0.,0.,19.5));
#27784=CARTESIAN_POINT('',(-2.86978283437093,0.00124690900571957,19.1339652973708));
#27785=CARTESIAN_POINT('Ctrl Pts',(-0.439445221994122,2.33068358199189,
19.62825));
#27786=CARTESIAN_POINT('Ctrl Pts',(-0.359496399915194,2.34930837340854,
19.6247608600375));
#27787=CARTESIAN_POINT('Ctrl Pts',(-0.278741728044194,2.36340753905626,
19.6212859488617));
#27788=CARTESIAN_POINT('Ctrl Pts',(-0.197506041411201,2.3731670460491,19.6178205395779));
#27789=CARTESIAN_POINT('Ctrl Pts',(-0.114116696920991,2.38318528956266,
19.6142632580364));
#27790=CARTESIAN_POINT('Ctrl Pts',(-0.0302197403964261,2.3886307553927,
19.6107159888789));
#27791=CARTESIAN_POINT('Ctrl Pts',(0.0538488183862894,2.38965232235862,
19.6071736192084));
#27792=CARTESIAN_POINT('Ctrl Pts',(0.0937194843833986,2.39013681449078,
19.6054936018509));
#27793=CARTESIAN_POINT('Ctrl Pts',(0.133628895976177,2.38962550572521,19.6038146865157));
#27794=CARTESIAN_POINT('Ctrl Pts',(0.173541591315785,2.3881303051021,19.6021363277883));
#27795=CARTESIAN_POINT('Ctrl Pts',(0.197736469304413,2.38722392189904,19.6011189150506));
#27796=CARTESIAN_POINT('Ctrl Pts',(0.221932555405085,2.38595593679589,19.600101706851));
#27797=CARTESIAN_POINT('Ctrl Pts',(0.246121926732615,2.38432855965558,19.5990845816929));
#27798=CARTESIAN_POINT('Ctrl Pts',(0.261966760970886,2.3832625740753,19.5984183312429));
#27799=CARTESIAN_POINT('Ctrl Pts',(0.27780950980444,2.38204221833013,19.5977520828035));
#27800=CARTESIAN_POINT('Ctrl Pts',(0.293631569537354,2.38066972871238,19.5970864910922));
#27801=CARTESIAN_POINT('Ctrl Pts',(0.379373845864251,2.37323198760618,19.5934795429833));
#27802=CARTESIAN_POINT('Ctrl Pts',(0.464621179595313,2.36132408278005,19.5898871205887));
#27803=CARTESIAN_POINT('Ctrl Pts',(0.549021293139782,2.3451096637313,19.5863039889554));
#27804=CARTESIAN_POINT('Ctrl Pts',(0.634164428857974,2.32875249993515,19.5826893129777));
#27805=CARTESIAN_POINT('Ctrl Pts',(0.718446312182276,2.30801251387993,19.5790840920651));
#27806=CARTESIAN_POINT('Ctrl Pts',(0.801504492173054,2.28300464467492,19.5754829517853));
#27807=CARTESIAN_POINT('Ctrl Pts',(0.853054825935946,2.26748342804869,19.5732478921756));
#27808=CARTESIAN_POINT('Ctrl Pts',(0.904133707598755,2.25031714023312,19.5710144044686));
#27809=CARTESIAN_POINT('Ctrl Pts',(0.954651843583393,2.23152350140498,19.5687812037332));
#27810=CARTESIAN_POINT('Ctrl Pts',(0.966661711293098,2.22705561850094,19.5682502964684));
#27811=CARTESIAN_POINT('Ctrl Pts',(0.978637539548016,2.22249655100818,19.5677195079304));
#27812=CARTESIAN_POINT('Ctrl Pts',(0.990570080353664,2.21784986361285,19.5671891810056));
#27813=CARTESIAN_POINT('Ctrl Pts',(1.07233004187525,2.18601146566952,19.5635554612747));
#27814=CARTESIAN_POINT('Ctrl Pts',(1.15216830046977,2.15002310442033,19.5599385463906));
#27815=CARTESIAN_POINT('Ctrl Pts',(1.22972588848851,2.11003339454853,19.5563331219261));
#27816=CARTESIAN_POINT('Ctrl Pts',(1.30689380941087,2.07024460214374,19.5527458119404));
#27817=CARTESIAN_POINT('Ctrl Pts',(1.3818048666458,2.02649428366031,19.5491698772035));
#27818=CARTESIAN_POINT('Ctrl Pts',(1.45409265027459,1.97887925509432,19.5456000829893));
#27819=CARTESIAN_POINT('Ctrl Pts',(1.51414958607928,1.93932052787409,19.542634285849));
#27820=CARTESIAN_POINT('Ctrl Pts',(1.57239588882887,1.89709330508863,19.5396727271079));
#27821=CARTESIAN_POINT('Ctrl Pts',(1.6286075594529,1.85222888403246,19.5367124049177));
#27822=CARTESIAN_POINT('Ctrl Pts',(1.65671339476491,1.82979667350437,19.5352322438226));
#27823=CARTESIAN_POINT('Ctrl Pts',(1.68431033399215,1.80670482947816,19.5337523918653));
#27824=CARTESIAN_POINT('Ctrl Pts',(1.71136870094884,1.78295531352429,19.5322724738146));
#27825=CARTESIAN_POINT('Ctrl Pts',(1.72505548280361,1.77094222919672,19.5315238951751));
#27826=CARTESIAN_POINT('Ctrl Pts',(1.7386044467155,1.7587608538397,19.5307752996251));
#27827=CARTESIAN_POINT('Ctrl Pts',(1.75201162231319,1.74641131895379,19.5300266386024));
#27828=CARTESIAN_POINT('Ctrl Pts',(1.76374413009413,1.73560434375724,19.5293714915723));
#27829=CARTESIAN_POINT('Ctrl Pts',(1.77536978940808,1.72466678187038,19.5287161918229));
#27830=CARTESIAN_POINT('Ctrl Pts',(1.78686993494738,1.71361443483951,19.5280616263465));
#27831=CARTESIAN_POINT('Ctrl Pts',(1.78820879329981,1.71232770963368,19.5279854211844));
#27832=CARTESIAN_POINT('Ctrl Pts',(1.7895459973299,1.71103938648239,19.527909223385));
#27833=CARTESIAN_POINT('Ctrl Pts',(1.79088154369118,1.70974946659003,19.5278330328994));
#27834=CARTESIAN_POINT('Ctrl Pts',(1.8509299108473,1.65175254072928,19.5244073830022));
#27835=CARTESIAN_POINT('Ctrl Pts',(1.90762953422213,1.59053155433168,19.5209965182257));
#27836=CARTESIAN_POINT('Ctrl Pts',(1.96096030440938,1.52647851758989,19.5175959868336));
#27837=CARTESIAN_POINT('Ctrl Pts',(2.01585595410063,1.46054597893928,19.514095673986));
#27838=CARTESIAN_POINT('Ctrl Pts',(2.06718257934786,1.39161216589875,19.5106063098428));
#27839=CARTESIAN_POINT('Ctrl Pts',(2.11488498779521,1.32006098590835,19.5071230391759));
#27840=CARTESIAN_POINT('Ctrl Pts',(2.16100614932092,1.25088159566155,19.5037552325118));
#27841=CARTESIAN_POINT('Ctrl Pts',(2.20373946041229,1.17925459387015,19.5003931220444));
#27842=CARTESIAN_POINT('Ctrl Pts',(2.24300118618815,1.10549836563141,19.4970323195431));
#27843=CARTESIAN_POINT('Ctrl Pts',(2.26017819121508,1.07323001577696,19.4955619684488));
#27844=CARTESIAN_POINT('Ctrl Pts',(2.27669026031943,1.04055381937119,19.4940918677074));
#27845=CARTESIAN_POINT('Ctrl Pts',(2.29252817853264,1.00749527125662,19.4926216498475));
#27846=CARTESIAN_POINT('Ctrl Pts',(2.300517169549,0.99081981932247,19.4918800399264));
#27847=CARTESIAN_POINT('Ctrl Pts',(2.30833460670403,0.974047072136536,19.4911384002056));
#27848=CARTESIAN_POINT('Ctrl Pts',(2.31597916990764,0.957180253262817,19.4903966835216));
#27849=CARTESIAN_POINT('Ctrl Pts',(2.32148143469363,0.945040160877076,19.4898628241652));
#27850=CARTESIAN_POINT('Ctrl Pts',(2.32689374255309,0.932852048460756,19.4893289576981));
#27851=CARTESIAN_POINT('Ctrl Pts',(2.332210604538,0.92062911548402,19.4887955857665));
#27852=CARTESIAN_POINT('Ctrl Pts',(2.36777326752894,0.838874116492736,19.4852280441781));
#27853=CARTESIAN_POINT('Ctrl Pts',(2.39913263839588,0.755425618458568,19.4816765201166));
#27854=CARTESIAN_POINT('Ctrl Pts',(2.4262333303409,0.670689801398847,19.4781359905495));
#27855=CARTESIAN_POINT('Ctrl Pts',(2.45364753630358,0.584973719093478,19.4745545024102));
#27856=CARTESIAN_POINT('Ctrl Pts',(2.47670437210413,0.497939463359003,19.4709842646162));
#27857=CARTESIAN_POINT('Ctrl Pts',(2.49530163963731,0.409978999236876,19.4674200777839));
#27858=CARTESIAN_POINT('Ctrl Pts',(2.51280420413611,0.327196209028843,19.4640656919955));
#27859=CARTESIAN_POINT('Ctrl Pts',(2.52635662496927,0.243592136482556,19.4607166657717));
#27860=CARTESIAN_POINT('Ctrl Pts',(2.53583313283201,0.159481833132225,19.457368664907));
#27861=CARTESIAN_POINT('Ctrl Pts',(2.53950882122587,0.126857656557172,19.4560700633441));
#27862=CARTESIAN_POINT('Ctrl Pts',(2.5425708637383,0.0941572581992666,19.4547716160424));
#27863=CARTESIAN_POINT('Ctrl Pts',(2.5450101915364,0.0613989272386214,19.4534730700835));
#27864=CARTESIAN_POINT('Ctrl Pts',(2.54664995154104,0.0393781881769477,
19.4526001641423));
#27865=CARTESIAN_POINT('Ctrl Pts',(2.54800830074101,0.0173312706195899,
19.4517272136201));
#27866=CARTESIAN_POINT('Ctrl Pts',(2.54908222580259,-0.00473625006357956,
19.4508541416904));
#27867=CARTESIAN_POINT('Ctrl Pts',(2.5497978073951,-0.0194403594638387,
19.450272393276));
#27868=CARTESIAN_POINT('Ctrl Pts',(2.55038670103113,-0.0341462169389561,
19.4496908837209));
#27869=CARTESIAN_POINT('Ctrl Pts',(2.55084824252384,-0.048844767938526,
19.4491098818334));
#27870=CARTESIAN_POINT('Ctrl Pts',(2.55374081608822,-0.140963549732027,
19.4454686258957));
#27871=CARTESIAN_POINT('Ctrl Pts',(2.55164005327307,-0.232884185733536,
19.4418437427226));
#27872=CARTESIAN_POINT('Ctrl Pts',(2.54444222542436,-0.324196175898947,
19.4382298881162));
#27873=CARTESIAN_POINT('Ctrl Pts',(2.53724439757566,-0.415508166064358,
19.4346160335098));
#27874=CARTESIAN_POINT('Ctrl Pts',(2.524949863139,-0.506212566736429,19.4310132074699));
#27875=CARTESIAN_POINT('Ctrl Pts',(2.50739898915578,-0.595905850588752,
19.4274160657988));
#27876=CARTESIAN_POINT('Ctrl Pts',(2.49041552541174,-0.682699399209003,
19.4239352177673));
#27877=CARTESIAN_POINT('Ctrl Pts',(2.46850979008406,-0.768546973818678,
19.4204596925007));
#27878=CARTESIAN_POINT('Ctrl Pts',(2.44195100957766,-0.853189635279847,
19.4169846475493));
#27879=CARTESIAN_POINT('Ctrl Pts',(2.43105026163653,-0.887930248367561,
19.4155583550624));
#27880=CARTESIAN_POINT('Ctrl Pts',(2.4193650665621,-0.922467728725974,19.4141321434892));
#27881=CARTESIAN_POINT('Ctrl Pts',(2.40691167793065,-0.956783357203964,
19.4127056780113));
#27882=CARTESIAN_POINT('Ctrl Pts',(2.40227529198214,-0.969559036370352,
19.4121746061325));
#27883=CARTESIAN_POINT('Ctrl Pts',(2.39753142734847,-0.982306537607564,
19.4116433912781));
#27884=CARTESIAN_POINT('Ctrl Pts',(2.39268420846545,-0.995016186464471,
19.4111123792872));
#27885=CARTESIAN_POINT('Ctrl Pts',(2.36008996603969,-1.08047991029981,19.4075416856628));
#27886=CARTESIAN_POINT('Ctrl Pts',(2.32289371031631,-1.16406508789994,19.4039871869403));
#27887=CARTESIAN_POINT('Ctrl Pts',(2.28145232389539,-1.2455084624321,19.4004438616248));
#27888=CARTESIAN_POINT('Ctrl Pts',(2.2401496080627,-1.3266793122823,19.3969123929349));
#27889=CARTESIAN_POINT('Ctrl Pts',(2.19462948656474,-1.40572341239688,19.3933920230006));
#27890=CARTESIAN_POINT('Ctrl Pts',(2.14519002651603,-1.48236812476013,19.3898777805668));
#27891=CARTESIAN_POINT('Ctrl Pts',(2.09545800359527,-1.5594663897543,19.3863427422575));
#27892=CARTESIAN_POINT('Ctrl Pts',(2.0417595663806,-1.63413758358452,19.3828139041835));
#27893=CARTESIAN_POINT('Ctrl Pts',(1.98435092675475,-1.70608041179627,19.3792862063132));
#27894=CARTESIAN_POINT('Ctrl Pts',(1.96385857271652,-1.73176083055963,19.3780269736581));
#27895=CARTESIAN_POINT('Ctrl Pts',(1.94289307887375,-1.75709333013408,19.376767886285));
#27896=CARTESIAN_POINT('Ctrl Pts',(1.92146486206384,-1.7820631761771,19.3755087140512));
#27897=CARTESIAN_POINT('Ctrl Pts',(1.90808270355052,-1.79765712133665,19.3747223470577));
#27898=CARTESIAN_POINT('Ctrl Pts',(1.89452006441996,-1.81310961476765,19.3739359469673));
#27899=CARTESIAN_POINT('Ctrl Pts',(1.88077936786051,-1.82841694049769,19.3731494577247));
#27900=CARTESIAN_POINT('Ctrl Pts',(1.8684512417402,-1.84215064325055,19.3724438211121));
#27901=CARTESIAN_POINT('Ctrl Pts',(1.85597675343054,-1.85577058254818,19.3717379474738));
#27902=CARTESIAN_POINT('Ctrl Pts',(1.84337723420589,-1.86925344146862,19.3710328821673));
#27903=CARTESIAN_POINT('Ctrl Pts',(1.77710288751082,-1.94017421634914,19.3673241896579));
#27904=CARTESIAN_POINT('Ctrl Pts',(1.70728117389982,-2.00741106239547,19.3636324635521));
#27905=CARTESIAN_POINT('Ctrl Pts',(1.63425481305677,-2.07065048051062,19.3599520680256));
#27906=CARTESIAN_POINT('Ctrl Pts',(1.56435178486444,-2.1311851528719,19.3564290827738));
#27907=CARTESIAN_POINT('Ctrl Pts',(1.4915113914409,-2.1880576143788,19.3529164796116));
#27908=CARTESIAN_POINT('Ctrl Pts',(1.4159918760443,-2.24096200122539,19.3494093153588));
#27909=CARTESIAN_POINT('Ctrl Pts',(1.34164349717693,-2.29304596093249,19.3459565392752));
#27910=CARTESIAN_POINT('Ctrl Pts',(1.26469778687837,-2.34128460563477,19.3425090347186));
#27911=CARTESIAN_POINT('Ctrl Pts',(1.18537076960009,-2.38534634059117,19.3390620849337));
#27912=CARTESIAN_POINT('Ctrl Pts',(1.15499487450069,-2.40221845660982,19.3377421791983));
#27913=CARTESIAN_POINT('Ctrl Pts',(1.12426954458043,-2.41847765262325,19.3364223548077));
#27914=CARTESIAN_POINT('Ctrl Pts',(1.0932060081487,-2.43410342660017,19.3351023469319));
#27915=CARTESIAN_POINT('Ctrl Pts',(1.07852356668983,-2.44148907994231,19.3344784341201));
#27916=CARTESIAN_POINT('Ctrl Pts',(1.06376556159054,-2.44873320670299,19.3338544803166));
#27917=CARTESIAN_POINT('Ctrl Pts',(1.04893314692695,-2.45583355114468,19.3332304575567));
#27918=CARTESIAN_POINT('Ctrl Pts',(1.03777451577937,-2.46117523868798,19.3327609965847));
#27919=CARTESIAN_POINT('Ctrl Pts',(1.02657507642648,-2.46643486915688,19.3322915524202));
#27920=CARTESIAN_POINT('Ctrl Pts',(1.01534417119219,-2.47160761026341,19.3318224792748));
#27921=CARTESIAN_POINT('Ctrl Pts',(0.976776596263432,-2.48937110092166,
19.3302116550977));
#27922=CARTESIAN_POINT('Ctrl Pts',(0.937809807627497,-2.50612368700867,
19.3286040154222));
#27923=CARTESIAN_POINT('Ctrl Pts',(0.898469638803505,-2.52183800942761,
19.3269990986982));
#27924=CARTESIAN_POINT('Ctrl Pts',(0.815541152704475,-2.55496356549997,
19.3236159583045));
#27925=CARTESIAN_POINT('Ctrl Pts',(0.730955270809804,-2.58347870238839,
19.3202449176199));
#27926=CARTESIAN_POINT('Ctrl Pts',(0.645080730189636,-2.60751906959201,
19.3168816532826));
#27927=CARTESIAN_POINT('Ctrl Pts',(0.556937627094779,-2.63219451530112,
19.3134295410143));
#27928=CARTESIAN_POINT('Ctrl Pts',(0.467436139325503,-2.65215578598813,
19.3099856213784));
#27929=CARTESIAN_POINT('Ctrl Pts',(0.376952220119887,-2.66749996206646,
19.3065452192493));
#27930=CARTESIAN_POINT('Ctrl Pts',(0.28814825433163,-2.68255925325844,19.3031686927278));
#27931=CARTESIAN_POINT('Ctrl Pts',(0.198397148537396,-2.69317110363349,
19.2997955543113));
#27932=CARTESIAN_POINT('Ctrl Pts',(0.108044784410401,-2.69938115345377,
19.2964213844691));
#27933=CARTESIAN_POINT('Ctrl Pts',(0.0846755836239938,-2.700987352722,19.2955486718037));
#27934=CARTESIAN_POINT('Ctrl Pts',(0.0612661467540061,-2.70229884783018,
19.2946758901386));
#27935=CARTESIAN_POINT('Ctrl Pts',(0.037822458411094,-2.7033159368433,19.2938029630042));
#27936=CARTESIAN_POINT('Ctrl Pts',(0.0220310773589827,-2.70400103553319,
19.2932149699884));
#27937=CARTESIAN_POINT('Ctrl Pts',(0.00623212385897853,-2.70455216083962,
19.2926272077515));
#27938=CARTESIAN_POINT('Ctrl Pts',(-0.00956443944047891,-2.70496967952273,
19.2920399533629));
#27939=CARTESIAN_POINT('Ctrl Pts',(-0.103598710039189,-2.70745509765341,
19.2885441272746));
#27940=CARTESIAN_POINT('Ctrl Pts',(-0.197635930615719,-2.70521413060483,
19.2850629827735));
#27941=CARTESIAN_POINT('Ctrl Pts',(-0.291281950672319,-2.69836938342123,
19.2815917980052));
#27942=CARTESIAN_POINT('Ctrl Pts',(-0.38606363263148,-2.69144162877396,
19.2780785175632));
#27943=CARTESIAN_POINT('Ctrl Pts',(-0.480445514899326,-2.67979776357681,
19.2745754398856));
#27944=CARTESIAN_POINT('Ctrl Pts',(-0.574027890122098,-2.66351219296258,
19.2710776692377));
#27945=CARTESIAN_POINT('Ctrl Pts',(-0.667261159572748,-2.64728737509896,
19.2675929469006));
#27946=CARTESIAN_POINT('Ctrl Pts',(-0.759701848049967,-2.62645531011172,
19.2641134920718));
#27947=CARTESIAN_POINT('Ctrl Pts',(-0.850949097824244,-2.60103852864063,
19.2606344636025));
#27948=CARTESIAN_POINT('Ctrl Pts',(-0.888409306005341,-2.59060404510764,
19.2592061999446));
#27949=CARTESIAN_POINT('Ctrl Pts',(-0.925668224932336,-2.57939626873602,
19.2577780081451));
#27950=CARTESIAN_POINT('Ctrl Pts',(-0.962697255759592,-2.56741431371771,
19.2563495532386));
#27951=CARTESIAN_POINT('Ctrl Pts',(-0.978584771163812,-2.56227338805281,
19.2557366665704));
#27952=CARTESIAN_POINT('Ctrl Pts',(-0.994429958507756,-2.55698992710178,
19.2551237314672));
#27953=CARTESIAN_POINT('Ctrl Pts',(-1.01023051820469,-2.55156378128263,
19.254510721472));
#27954=CARTESIAN_POINT('Ctrl Pts',(-1.02485107054566,-2.54654286743652,
19.2539434918995));
#27955=CARTESIAN_POINT('Ctrl Pts',(-1.03942581785439,-2.54140235120542,
19.2533764922911));
#27956=CARTESIAN_POINT('Ctrl Pts',(-1.05394656826891,-2.53614492416381,
19.2528099559783));
#27957=CARTESIAN_POINT('Ctrl Pts',(-1.1442425835919,-2.5034520743346,19.2492869995111));
#27958=CARTESIAN_POINT('Ctrl Pts',(-1.23253047867916,-2.46621543590235,
19.2457788737934));
#27959=CARTESIAN_POINT('Ctrl Pts',(-1.31841054501642,-2.42451396270994,
19.2422807482851));
#27960=CARTESIAN_POINT('Ctrl Pts',(-1.40295505543142,-2.38346100612755,
19.2388370235527));
#27961=CARTESIAN_POINT('Ctrl Pts',(-1.48516695569074,-2.33808077848995,
19.2354029904136));
#27962=CARTESIAN_POINT('Ctrl Pts',(-1.56465265588408,-2.28840031795577,
19.2319740402064));
#27963=CARTESIAN_POINT('Ctrl Pts',(-1.60634279285186,-2.26234298689805,
19.2301755606881));
#27964=CARTESIAN_POINT('Ctrl Pts',(-1.64728266840485,-2.23510188014699,
19.2283784794781));
#27965=CARTESIAN_POINT('Ctrl Pts',(-1.68741284053105,-2.20667575559394,
19.2265821315976));
#27966=CARTESIAN_POINT('Ctrl Pts',(-1.76408500272364,-2.15236518783998,
19.2231500537182));
#27967=CARTESIAN_POINT('Ctrl Pts',(-1.83780366664609,-2.09373114303323,
19.2197206527414));
#27968=CARTESIAN_POINT('Ctrl Pts',(-1.90842406585113,-2.03112180178175,
19.2162892909117));
#27969=CARTESIAN_POINT('Ctrl Pts',(-1.92415367580141,-2.01717653202662,
19.2155250077331));
#27970=CARTESIAN_POINT('Ctrl Pts',(-1.93973411950598,-2.0030293780058,19.2147603912815));
#27971=CARTESIAN_POINT('Ctrl Pts',(-1.95513815612309,-1.98870805072037,
19.2139966607035));
#27972=CARTESIAN_POINT('Ctrl Pts',(-2.02393936909849,-1.92474269455126,
19.2105855035206));
#27973=CARTESIAN_POINT('Ctrl Pts',(-2.08930100738169,-1.85724208008421,
19.2071883480391));
#27974=CARTESIAN_POINT('Ctrl Pts',(-2.15113215444763,-1.78661473678416,
19.2038008153795));
#27975=CARTESIAN_POINT('Ctrl Pts',(-2.21426051930702,-1.714505631447,19.2003422122668));
#27976=CARTESIAN_POINT('Ctrl Pts',(-2.27370921946588,-1.63913657767921,
19.1968936399852));
#27977=CARTESIAN_POINT('Ctrl Pts',(-2.32934945775057,-1.56089671412961,
19.1934504382259));
#27978=CARTESIAN_POINT('Ctrl Pts',(-2.3854816519556,-1.48196507489273,19.189976792609));
#27979=CARTESIAN_POINT('Ctrl Pts',(-2.43773825193628,-1.40011084488009,
19.1865086129037));
#27980=CARTESIAN_POINT('Ctrl Pts',(-2.48594698643214,-1.31569866499581,
19.1830411140891));
#27981=CARTESIAN_POINT('Ctrl Pts',(-2.51310393228564,-1.26814759313163,
19.1810878025463));
#27982=CARTESIAN_POINT('Ctrl Pts',(-2.53897560819788,-1.21978424599781,
19.1791347070703));
#27983=CARTESIAN_POINT('Ctrl Pts',(-2.56352474874957,-1.17067045541336,
19.1771809723));
#27984=CARTESIAN_POINT('Ctrl Pts',(-2.5701220073907,-1.15747177016204,19.1766559317769));
#27985=CARTESIAN_POINT('Ctrl Pts',(-2.57662472903377,-1.14421678676666,
19.1761307625987));
#27986=CARTESIAN_POINT('Ctrl Pts',(-2.58302887965335,-1.13091345079126,
19.1756057150565));
#27987=CARTESIAN_POINT('Ctrl Pts',(-2.62568677355004,-1.04230024847588,
19.172108385953));
#27988=CARTESIAN_POINT('Ctrl Pts',(-2.66385866655196,-0.951788919503196,
19.1686260589889));
#27989=CARTESIAN_POINT('Ctrl Pts',(-2.69741818565158,-0.859782121332853,
19.1651540264633));
#27990=CARTESIAN_POINT('Ctrl Pts',(-2.73103699790175,-0.767612765024542,
19.1616758595307));
#27991=CARTESIAN_POINT('Ctrl Pts',(-2.76002758078427,-0.673941779287795,
19.1582080234452));
#27992=CARTESIAN_POINT('Ctrl Pts',(-2.78421958380913,-0.579144596406193,
19.1547457855091));
#27993=CARTESIAN_POINT('Ctrl Pts',(-2.80790962022943,-0.486314386658796,
19.1513553865116));
#27994=CARTESIAN_POINT('Ctrl Pts',(-2.82699841437237,-0.392403361685435,
19.1479703557585));
#27995=CARTESIAN_POINT('Ctrl Pts',(-2.84127941192308,-0.297748919984249,
19.1445862490817));
#27996=CARTESIAN_POINT('Ctrl Pts',(-2.85260005450855,-0.222715708906352,
19.1419036450113));
#27997=CARTESIAN_POINT('Ctrl Pts',(-2.86089874028508,-0.147214912387106,
19.1392216216156));
#27998=CARTESIAN_POINT('Ctrl Pts',(-2.8660492635332,-0.0714129213286235,
19.1365379651471));
#27999=CARTESIAN_POINT('Ctrl Pts',(-2.86769679090258,-0.0471657043165984,
19.1356795285827));
#28000=CARTESIAN_POINT('Ctrl Pts',(-2.8690199678599,-0.0229179339290668,
19.1348219958471));
#28001=CARTESIAN_POINT('Ctrl Pts',(-2.87001662176841,0.00132468418317613,
19.1339652973708));
#28002=CARTESIAN_POINT('',(0.261007814359831,2.92578301259841,19.058));
#28003=CARTESIAN_POINT('Ctrl Pts',(0.260898964428293,2.92506788491831,19.058));
#28004=CARTESIAN_POINT('Ctrl Pts',(0.163023909524402,2.92122872644259,19.0703782857669));
#28005=CARTESIAN_POINT('Ctrl Pts',(0.0656137074299065,2.912742505651,19.0828007237738));
#28006=CARTESIAN_POINT('Ctrl Pts',(-0.030953795983259,2.89962093163934,
19.0952868597003));
#28007=CARTESIAN_POINT('Ctrl Pts',(-0.130391850521096,2.88610930768639,
19.1081441566308));
#28008=CARTESIAN_POINT('Ctrl Pts',(-0.228937522172488,2.86768264892189,
19.1210689947157));
#28009=CARTESIAN_POINT('Ctrl Pts',(-0.326154050402428,2.8443004424986,19.134082714997));
#28010=CARTESIAN_POINT('Ctrl Pts',(-0.399066446574882,2.82676378768113,
19.143843005208));
#28011=CARTESIAN_POINT('Ctrl Pts',(-0.471230789680895,2.80643850217304,
19.1536532916545));
#28012=CARTESIAN_POINT('Ctrl Pts',(-0.542448327672379,2.78328892000252,
19.1635225775885));
#28013=CARTESIAN_POINT('Ctrl Pts',(-0.595861481165992,2.76592673337463,
19.1709245420391));
#28014=CARTESIAN_POINT('Ctrl Pts',(-0.6487418158016,2.74697554899712,19.1783596937014));
#28015=CARTESIAN_POINT('Ctrl Pts',(-0.700999502826955,2.72641481549739,
19.1858318308225));
#28016=CARTESIAN_POINT('Ctrl Pts',(-0.716250316273543,2.72041439854864,
19.1880124893202));
#28017=CARTESIAN_POINT('Ctrl Pts',(-0.731448062028104,2.71427686698661,
19.1901962978622));
#28018=CARTESIAN_POINT('Ctrl Pts',(-0.746590412830255,2.70800163764602,
19.1923833508571));
#28019=CARTESIAN_POINT('Ctrl Pts',(-0.759834193701528,2.70251320567204,
19.1942961879718));
#28020=CARTESIAN_POINT('Ctrl Pts',(-0.773030676312604,2.69692143623512,
19.1962107991778));
#28021=CARTESIAN_POINT('Ctrl Pts',(-0.786171449556019,2.69122928513894,
19.1981262233848));
#28022=CARTESIAN_POINT('Ctrl Pts',(-0.869595052331544,2.65509292214185,
19.2102862070654));
#28023=CARTESIAN_POINT('Ctrl Pts',(-0.950864331706193,2.61487768287787,
19.2224917235733));
#28024=CARTESIAN_POINT('Ctrl Pts',(-1.02964582077395,2.5705582476779,19.2347617221928));
#28025=CARTESIAN_POINT('Ctrl Pts',(-1.070119428365,2.54778935297729,19.2410653744231));
#28026=CARTESIAN_POINT('Ctrl Pts',(-1.1099359371769,2.52393656066965,19.2473860456799));
#28027=CARTESIAN_POINT('Ctrl Pts',(-1.14904652243468,2.49899242632004,19.2537263053885));
#28028=CARTESIAN_POINT('Ctrl Pts',(-1.22710174167599,2.4492099988107,19.2663799222633));
#28029=CARTESIAN_POINT('Ctrl Pts',(-1.30234807687636,2.39508206632693,19.2791115608326));
#28030=CARTESIAN_POINT('Ctrl Pts',(-1.37457154418326,2.3369356258057,19.291941645948));
#28031=CARTESIAN_POINT('Ctrl Pts',(-1.44877133871285,2.27719806265369,19.3051228142698));
#28032=CARTESIAN_POINT('Ctrl Pts',(-1.5197812312985,2.21321803485081,19.3184078906476));
#28033=CARTESIAN_POINT('Ctrl Pts',(-1.58731554407866,2.14533092033585,19.3318190229539));
#28034=CARTESIAN_POINT('Ctrl Pts',(-1.59783038643963,2.1347611480515,19.3339070865807));
#28035=CARTESIAN_POINT('Ctrl Pts',(-1.60826086139227,2.12409664410853,19.3359982059718));
#28036=CARTESIAN_POINT('Ctrl Pts',(-1.61860576158074,2.11333865957609,19.3380924647195));
#28037=CARTESIAN_POINT('Ctrl Pts',(-1.62822431541569,2.10333602528327,19.3400396793027));
#28038=CARTESIAN_POINT('Ctrl Pts',(-1.63776282721144,2.09325885830216,19.341988383369));
#28039=CARTESIAN_POINT('Ctrl Pts',(-1.64721859595761,2.08311066413915,19.343938216497));
#28040=CARTESIAN_POINT('Ctrl Pts',(-1.70843622698655,2.01741019889329,19.3565616391085));
#28041=CARTESIAN_POINT('Ctrl Pts',(-1.766219100483,1.9487041025178,19.3692383719282));
#28042=CARTESIAN_POINT('Ctrl Pts',(-1.82039858689206,1.87731348025079,19.3819900850371));
#28043=CARTESIAN_POINT('Ctrl Pts',(-1.87433752519525,1.80623982073302,19.3946851826143));
#28044=CARTESIAN_POINT('Ctrl Pts',(-1.92470528964026,1.73250442333618,19.407454596158));
#28045=CARTESIAN_POINT('Ctrl Pts',(-1.97128720650435,1.65640691870135,19.4203197083937));
#28046=CARTESIAN_POINT('Ctrl Pts',(-2.01705756114674,1.58163520450376,19.4329606813117));
#28047=CARTESIAN_POINT('Ctrl Pts',(-2.05917296516592,1.50458207736984,19.4456940473948));
#28048=CARTESIAN_POINT('Ctrl Pts',(-2.09738014456683,1.42552910739471,19.4585400911205));
#28049=CARTESIAN_POINT('Ctrl Pts',(-2.1193437171634,1.3800851444472,19.465924698369));
#28050=CARTESIAN_POINT('Ctrl Pts',(-2.14001485636328,1.33398034007164,19.4733465408239));
#28051=CARTESIAN_POINT('Ctrl Pts',(-2.15933758201886,1.28726947129132,19.4808094718297));
#28052=CARTESIAN_POINT('Ctrl Pts',(-2.16497166515239,1.27364960613157,19.4829854988797));
#28053=CARTESIAN_POINT('Ctrl Pts',(-2.17049154787065,1.2599767962587,19.4851652437125));
#28054=CARTESIAN_POINT('Ctrl Pts',(-2.17588921595073,1.2462696637705,19.4873460678037));
#28055=CARTESIAN_POINT('Ctrl Pts',(-2.20705516631138,1.16712515092234,19.4999380713062));
#28056=CARTESIAN_POINT('Ctrl Pts',(-2.23420478857045,1.0867091474059,19.5125864882835));
#28057=CARTESIAN_POINT('Ctrl Pts',(-2.25715829612839,1.0052897707403,19.5253134008472));
#28058=CARTESIAN_POINT('Ctrl Pts',(-2.27976324370209,0.925106786228536,
19.53784704916));
#28059=CARTESIAN_POINT('Ctrl Pts',(-2.29829861115926,0.843949859450999,
19.5504568271743));
#28060=CARTESIAN_POINT('Ctrl Pts',(-2.31254304095193,0.762077696140832,
19.5631638262184));
#28061=CARTESIAN_POINT('Ctrl Pts',(-2.32637402815749,0.682581860946577,
19.5755020063884));
#28062=CARTESIAN_POINT('Ctrl Pts',(-2.33615945602606,0.602411077429613,
19.5879318458378));
#28063=CARTESIAN_POINT('Ctrl Pts',(-2.3416499618205,0.521815068187646,19.6004726521654));
#28064=CARTESIAN_POINT('Ctrl Pts',(-2.34567646704228,0.462709356579674,
19.6096695502389));
#28065=CARTESIAN_POINT('Ctrl Pts',(-2.34739215247365,0.403375179185436,
19.6189261278148));
#28066=CARTESIAN_POINT('Ctrl Pts',(-2.34668236863853,0.34391848339548,19.62825));
#28067=CARTESIAN_POINT('',(-2.14350474087485,2.01162918712768,19.058));
#28068=CARTESIAN_POINT('Origin',(0.,0.,19.058));
#28069=CARTESIAN_POINT('Ctrl Pts',(-2.87001662176841,0.00132468418317613,
19.1339652973708));
#28070=CARTESIAN_POINT('Ctrl Pts',(-2.8730496525982,0.0751001517771462,
19.1313581808297));
#28071=CARTESIAN_POINT('Ctrl Pts',(-2.87305989114646,0.14882755829897,19.1287587900596));
#28072=CARTESIAN_POINT('Ctrl Pts',(-2.86997577113599,0.222349839512856,
19.126165164497));
#28073=CARTESIAN_POINT('Ctrl Pts',(-2.86597654860783,0.317687233114156,
19.1228019731347));
#28074=CARTESIAN_POINT('Ctrl Pts',(-2.85677656440916,0.412680012263468,
19.1194484757843));
#28075=CARTESIAN_POINT('Ctrl Pts',(-2.84265033724356,0.507029984461914,
19.1161003976653));
#28076=CARTESIAN_POINT('Ctrl Pts',(-2.82824071780026,0.603272751757619,
19.1126851523209));
#28077=CARTESIAN_POINT('Ctrl Pts',(-2.80870497678361,0.6988474329182,19.1092755458241));
#28078=CARTESIAN_POINT('Ctrl Pts',(-2.784279579828,0.793434685907145,19.1058670409239));
#28079=CARTESIAN_POINT('Ctrl Pts',(-2.76987697537351,0.849208714624576,
19.1038571924065));
#28080=CARTESIAN_POINT('Ctrl Pts',(-2.75377324450372,0.90463930914618,19.1018477269091));
#28081=CARTESIAN_POINT('Ctrl Pts',(-2.73600874080969,0.959658848626435,
19.0998377142003));
#28082=CARTESIAN_POINT('Ctrl Pts',(-2.72986209641136,0.978695999901232,
19.0991422355328));
#28083=CARTESIAN_POINT('Ctrl Pts',(-2.72351657272334,0.9976839197633,19.0984466913527));
#28084=CARTESIAN_POINT('Ctrl Pts',(-2.71697368591159,1.01661973836998,19.0977510431258));
#28085=CARTESIAN_POINT('Ctrl Pts',(-2.71223360146931,1.03033805289415,19.0972470711891));
#28086=CARTESIAN_POINT('Ctrl Pts',(-2.70738997743942,1.04402867625674,19.0967430566156));
#28087=CARTESIAN_POINT('Ctrl Pts',(-2.70244828698933,1.05767755042078,19.0962394649656));
#28088=CARTESIAN_POINT('Ctrl Pts',(-2.66878296987175,1.15066064632101,19.0928087416602));
#28089=CARTESIAN_POINT('Ctrl Pts',(-2.6305179809939,1.24186163011973,19.0893919514575));
#28090=CARTESIAN_POINT('Ctrl Pts',(-2.58793978625899,1.33096685230041,19.0859846442085));
#28091=CARTESIAN_POINT('Ctrl Pts',(-2.54484291834037,1.42115752419453,19.0825358302938));
#28092=CARTESIAN_POINT('Ctrl Pts',(-2.49732675054846,1.50920190161696,19.0790967317763));
#28093=CARTESIAN_POINT('Ctrl Pts',(-2.4456353402102,1.59476406879245,19.0756627338873));
#28094=CARTESIAN_POINT('Ctrl Pts',(-2.3941166019357,1.68004042066733,19.0722402070628));
#28095=CARTESIAN_POINT('Ctrl Pts',(-2.33844998117206,1.76285193805007,19.068822746847));
#28096=CARTESIAN_POINT('Ctrl Pts',(-2.27883141277619,1.84284311864553,19.065405784563));
#28097=CARTESIAN_POINT('Ctrl Pts',(-2.23576527783441,1.90062563624645,19.062937503912));
#28098=CARTESIAN_POINT('Ctrl Pts',(-2.19063602623153,1.95693605387978,19.0604694830846));
#28099=CARTESIAN_POINT('Ctrl Pts',(-2.14350474087485,2.01162918712768,19.058));
#28100=CARTESIAN_POINT('',(-2.,-2.44929359829471E-16,20.));
#28101=CARTESIAN_POINT('',(-2.5,-3.06161699786838E-16,19.5));
#28102=CARTESIAN_POINT('Origin',(0.,0.,20.));
#28103=CARTESIAN_POINT('Ctrl Pts',(1.70810875200395,-2.39535560853238,-0.329233991005387));
#28104=CARTESIAN_POINT('Ctrl Pts',(2.50223308968789,-1.82907195255014,-0.276469878102161));
#28105=CARTESIAN_POINT('Ctrl Pts',(3.46973755032763,0.145306414888747,-0.170941652295709));
#28106=CARTESIAN_POINT('Ctrl Pts',(1.76544499098352,2.99434248509872,-0.0126493135860318));
#28107=CARTESIAN_POINT('Ctrl Pts',(-1.54740154846188,3.1089951954401,0.145643025123646));
#28108=CARTESIAN_POINT('Ctrl Pts',(-3.45088210452873,0.39789687314801,0.303935363833323));
#28109=CARTESIAN_POINT('Ctrl Pts',(-2.21346936403042,-2.67765081270084,
0.462227702543001));
#28110=CARTESIAN_POINT('Ctrl Pts',(1.03905693981445,-3.31458536367054,0.620520041252677));
#28111=CARTESIAN_POINT('Ctrl Pts',(3.34562773737951,-0.934901086274263,
0.778812379962355));
#28112=CARTESIAN_POINT('Ctrl Pts',(2.60676621014795,2.2961361704366,0.937104718672033));
#28113=CARTESIAN_POINT('Ctrl Pts',(-0.505039165470731,3.43685521821756,
1.09539705738171));
#28114=CARTESIAN_POINT('Ctrl Pts',(-3.15709632883502,1.44912788777876,1.25368939609139));
#28115=CARTESIAN_POINT('Ctrl Pts',(-2.93528897896573,-1.85777219083972,
1.41198173480107));
#28116=CARTESIAN_POINT('Ctrl Pts',(-0.0415132245718345,-3.47353675349846,
1.57027407351074));
#28117=CARTESIAN_POINT('Ctrl Pts',(2.89004928033421,-1.9273884963075,1.72856641222042));
#28118=CARTESIAN_POINT('Ctrl Pts',(3.19083026616817,1.37324872519892,1.8868587509301));
#28119=CARTESIAN_POINT('Ctrl Pts',(0.587029982052427,3.42382799431733,2.04515108963977));
#28120=CARTESIAN_POINT('Ctrl Pts',(-2.55113744546929,2.35773296697854,2.20344342834945));
#28121=CARTESIAN_POINT('Ctrl Pts',(-3.36703034140273,-0.854583572490759,
2.36173576705913));
#28122=CARTESIAN_POINT('Ctrl Pts',(-1.11794935940593,-3.28898079903561,
2.52002810576881));
#28123=CARTESIAN_POINT('Ctrl Pts',(2.14878960983019,-2.72945221239069,2.67832044447848));
#28124=CARTESIAN_POINT('Ctrl Pts',(3.45950707796974,0.314669352524756,2.83661278318816));
#28125=CARTESIAN_POINT('Ctrl Pts',(1.6210701051072,3.072350505369,2.99490512189784));
#28126=CARTESIAN_POINT('Ctrl Pts',(-1.69301064028636,3.0333019941398,3.15319746060751));
#28127=CARTESIAN_POINT('Ctrl Pts',(-3.46596086572504,0.233069227837938,
3.3114897993172));
#28128=CARTESIAN_POINT('Ctrl Pts',(-2.08388184344624,-2.77932409737199,
3.46978213802687));
#28129=CARTESIAN_POINT('Ctrl Pts',(1.19513381840354,-3.26172671239436,3.62807447673655));
#28130=CARTESIAN_POINT('Ctrl Pts',(3.38623121053353,-0.775012370246788,
3.78636681544623));
#28131=CARTESIAN_POINT('Ctrl Pts',(2.49487645815869,2.41718792041892,3.9446591541559));
#28132=CARTESIAN_POINT('Ctrl Pts',(-0.667539190367716,3.40904640851925,
4.10295149286558));
#28133=CARTESIAN_POINT('Ctrl Pts',(-3.22230064149105,1.29768430718665,4.26124383157526));
#28134=CARTESIAN_POINT('Ctrl Pts',(-2.84383429323506,-1.99494674059711,
4.41953617028494));
#28135=CARTESIAN_POINT('Ctrl Pts',(0.123345751738387,-3.47159787576266,
4.57782850899461));
#28136=CARTESIAN_POINT('Ctrl Pts',(2.97824540200357,-1.78808845160989,4.73612084770429));
#28137=CARTESIAN_POINT('Ctrl Pts',(3.12207827781955,1.52309986951151,4.89441318641397));
#28138=CARTESIAN_POINT('Ctrl Pts',(0.42391476189898,3.44782572935734,5.05270552512364));
#28139=CARTESIAN_POINT('Ctrl Pts',(-2.66013408953218,2.2340305752299,5.21099786383333));
#28140=CARTESIAN_POINT('Ctrl Pts',(-3.32268968830985,-1.01338009678248,
5.36929020254299));
#28141=CARTESIAN_POINT('Ctrl Pts',(-0.960634350157316,-3.33832107962339,
5.52758254125269));
#28142=CARTESIAN_POINT('Ctrl Pts',(2.27587675559227,-2.62442202755419,5.68587487996235));
#28143=CARTESIAN_POINT('Ctrl Pts',(3.44068018719777,0.478461947057601,5.84416721867204));
#28144=CARTESIAN_POINT('Ctrl Pts',(1.47346711985291,3.14580683324172,6.0024595573817));
#28145=CARTESIAN_POINT('Ctrl Pts',(-1.8350282169722,2.94955546282373,6.1607518960914));
#28146=CARTESIAN_POINT('Ctrl Pts',(-3.47311586145163,0.0683534804580524,
6.31904423480106));
#28147=CARTESIAN_POINT('Ctrl Pts',(-1.94966113959674,-2.87506998629669,
6.47733657351074));
#28148=CARTESIAN_POINT('Ctrl Pts',(1.34855046878899,-3.20134621971548,6.63562891222042));
#28149=CARTESIAN_POINT('Ctrl Pts',(3.41919017623777,-0.61346925275575,6.7939212509301));
#28150=CARTESIAN_POINT('Ctrl Pts',(2.37737552513495,2.53284259239435,6.95221358963977));
#28151=CARTESIAN_POINT('Ctrl Pts',(-0.828540107113662,3.37353335188222,
7.11050592834946));
#28152=CARTESIAN_POINT('Ctrl Pts',(-3.28024402995153,1.14333069989614,7.26879826705912));
#28153=CARTESIAN_POINT('Ctrl Pts',(-2.74597487089154,-2.12763436562531,
7.42709060576881));
#28154=CARTESIAN_POINT('Ctrl Pts',(0.287927538982181,-3.46183531059079,
7.58538294447848));
#28155=CARTESIAN_POINT('Ctrl Pts',(3.05973241187765,-1.64476246098426,7.74367528318817));
#28156=CARTESIAN_POINT('Ctrl Pts',(3.04629370647385,1.66952108080595,7.90196762189784));
#28157=CARTESIAN_POINT('Ctrl Pts',(0.259844540863475,3.46405640830819,8.06025996060752));
#28158=CARTESIAN_POINT('Ctrl Pts',(-2.76313849156042,2.10529609837068,8.21855229931719));
#28159=CARTESIAN_POINT('Ctrl Pts',(-3.27086440225209,-1.16989403256776,
8.37684463802688));
#28160=CARTESIAN_POINT('Ctrl Pts',(-0.801155411612067,-3.38014141594732,
8.53513697673654));
#28161=CARTESIAN_POINT('Ctrl Pts',(2.39783727610882,-2.51348013373106,8.69342931544623));
#28162=CARTESIAN_POINT('Ctrl Pts',(3.41410285698758,0.641176783162679,8.8517216541559));
#28163=CARTESIAN_POINT('Ctrl Pts',(1.32254501475776,3.21217693617538,9.01001399286559));
#28164=CARTESIAN_POINT('Ctrl Pts',(-1.97291222568947,2.85916479676892,9.16830633157525));
#28165=CARTESIAN_POINT('Ctrl Pts',(-3.47244735026198,-0.0965162422401203,
9.32659867028495));
#28166=CARTESIAN_POINT('Ctrl Pts',(-1.81104864749881,-2.96433951863654,
9.4848910089946));
#28167=CARTESIAN_POINT('Ctrl Pts',(1.49892938718647,-3.13375440607372,9.6431833477043));
#28168=CARTESIAN_POINT('Ctrl Pts',(3.44444710704859,-0.45054423989462,9.80147568641397));
#28169=CARTESIAN_POINT('Ctrl Pts',(2.25451933878342,2.64279180723891,9.95976802512365));
#28170=CARTESIAN_POINT('Ctrl Pts',(-0.987674662346407,3.3304211065144,10.1180603638333));
#28171=CARTESIAN_POINT('Ctrl Pts',(-3.33079837220816,0.986401636785503,
10.276352702543));
#28172=CARTESIAN_POINT('Ctrl Pts',(-2.64192989190662,-2.25552930187303,
10.4346450412527));
#28173=CARTESIAN_POINT('Ctrl Pts',(0.45186074341242,-3.44427464844491,10.5929373799624));
#28174=CARTESIAN_POINT('Ctrl Pts',(3.13432709789262,-1.49773149421841,10.751229718672));
#28175=CARTESIAN_POINT('Ctrl Pts',(2.96364708316543,1.81218154493491,10.9095220573817));
#28176=CARTESIAN_POINT('Ctrl Pts',(0.0951889965099087,3.47248398704746,
11.0678143960914));
#28177=CARTESIAN_POINT('Ctrl Pts',(-2.85991867434608,1.97181925172773,11.2261067348011));
#28178=CARTESIAN_POINT('Ctrl Pts',(-3.21167119843867,-1.32377267628441,
11.3843990735108));
#28179=CARTESIAN_POINT('Ctrl Pts',(-0.639871798076946,-3.41434767816393,
11.5426914122204));
#28180=CARTESIAN_POINT('Ctrl Pts',(2.514396451394,-2.39687639868534,11.7009837509301));
#28181=CARTESIAN_POINT('Ctrl Pts',(3.37983495145364,0.802447310600554,11.8592760896398));
#28182=CARTESIAN_POINT('Ctrl Pts',(1.16864375745746,3.27131132017627,12.0175684283495));
#28183=CARTESIAN_POINT('Ctrl Pts',(-2.10635207126507,2.76233360353794,12.1758607670591));
#28184=CARTESIAN_POINT('Ctrl Pts',(-3.46395683750307,-0.261168553377433,
12.3341531057688));
#28185=CARTESIAN_POINT('Ctrl Pts',(-1.66835660460176,-3.04693160823137,
12.4924454444785));
#28186=CARTESIAN_POINT('Ctrl Pts',(1.64593183163456,-3.05910352733767,12.6507377831882));
#28187=CARTESIAN_POINT('Ctrl Pts',(3.4619451093692,-0.286604335403503,12.8090301218978));
#28188=CARTESIAN_POINT('Ctrl Pts',(2.1265846438105,2.74678789462661,12.9673224606075));
#28189=CARTESIAN_POINT('Ctrl Pts',(-1.14458439111546,3.27980678653062,13.1256147993172));
#28190=CARTESIAN_POINT('Ctrl Pts',(-3.37384979002366,0.827250614816437,
13.2839071380269));
#28191=CARTESIAN_POINT('Ctrl Pts',(-2.53193372700732,-2.37834345446631,
13.4421994767365));
#28192=CARTESIAN_POINT('Ctrl Pts',(0.614776090670012,-3.41895544628708,
13.6004918154462));
#28193=CARTESIAN_POINT('Ctrl Pts',(3.20186142877222,-1.34732675186611,13.7587841541559));
#28194=CARTESIAN_POINT('Ctrl Pts',(2.87432457688735,1.95075990631232,13.9170764928656));
#28195=CARTESIAN_POINT('Ctrl Pts',(-0.0696809696671145,3.47308948168699,
14.0753688315753));
#28196=CARTESIAN_POINT('Ctrl Pts',(-2.95025663177125,1.83390070397115,14.2336611702849));
#28197=CARTESIAN_POINT('Ctrl Pts',(-3.14524341492572,-1.47466940238759,
14.3919535089946));
#28198=CARTESIAN_POINT('Ctrl Pts',(-0.477146815446115,-3.44086281355539,
14.5502458477043));
#28199=CARTESIAN_POINT('Ctrl Pts',(2.62529172131977,-2.27487348290887,14.708538186414));
#28200=CARTESIAN_POINT('Ctrl Pts',(3.33795366224388,0.961910253000547,14.8668305251236));
#28201=CARTESIAN_POINT('Ctrl Pts',(1.01211002426958,3.32307677956238,15.0251228638333));
#28202=CARTESIAN_POINT('Ctrl Pts',(-2.23504716804512,2.65928000440727,15.183415202543));
#28203=CARTESIAN_POINT('Ctrl Pts',(-3.44766344946911,-0.425232559234952,
15.3417075412527));
#28204=CARTESIAN_POINT('Ctrl Pts',(-1.52190643639689,-3.12266020798474,
15.4999998799623));
#28205=CARTESIAN_POINT('Ctrl Pts',(1.78922666348011,-2.97756174317077,15.658292218672));
#28206=CARTESIAN_POINT('Ctrl Pts',(3.47164477187003,-0.122018825280182,
15.8165845573817));
#28207=CARTESIAN_POINT('Ctrl Pts',(1.99385961608439,2.84459658736723,15.9748768960914));
#28208=CARTESIAN_POINT('Ctrl Pts',(-1.29891582365465,3.22180441786908,16.1331692348011));
#28209=CARTESIAN_POINT('Ctrl Pts',(-3.40930133753709,0.666236111980054,
16.2914615735107));
#28210=CARTESIAN_POINT('Ctrl Pts',(-2.4162340926357,-2.49580012745533,16.4497539122204));
#28211=CARTESIAN_POINT('Ctrl Pts',(0.776306484896849,-3.3859348256877,16.6080462509301));
#28212=CARTESIAN_POINT('Ctrl Pts',(3.26218349561107,-1.19388686658981,16.7663385896398));
#28213=CARTESIAN_POINT('Ctrl Pts',(2.77852697784647,2.08494368458209,16.9246309283494));
#28214=CARTESIAN_POINT('Ctrl Pts',(-0.234393177244862,3.46587213947896,
17.0829232670591));
#28215=CARTESIAN_POINT('Ctrl Pts',(-3.03395038925589,1.69184996202172,17.2412156057688));
#28216=CARTESIAN_POINT('Ctrl Pts',(-3.0717277841222,-1.62224207378881,17.3995079444785));
#28217=CARTESIAN_POINT('Ctrl Pts',(-0.313352558263224,-3.45963134991648,
17.5578002831882));
#28218=CARTESIAN_POINT('Ctrl Pts',(2.73028386654254,-2.14773808290938,17.7160926218978));
#28219=CARTESIAN_POINT('Ctrl Pts',(3.28853312351893,1.11919088861887,17.8743849606075));
#28220=CARTESIAN_POINT('Ctrl Pts',(0.853335008049955,3.36738633833314,18.0326772993172));
#28221=CARTESIAN_POINT('Ctrl Pts',(-2.35878130152261,2.55017955638957,18.1909696380269));
#28222=CARTESIAN_POINT('Ctrl Pts',(-3.42346318292819,-0.58823064555564,
18.3492619767365));
#28223=CARTESIAN_POINT('Ctrl Pts',(-1.3722967672463,-3.19156107302743,18.5075543154462));
#28224=CARTESIAN_POINT('Ctrl Pts',(1.92900469321343,-2.88891850258502,18.6658466541559));
#28225=CARTESIAN_POINT('Ctrl Pts',(3.47253961472093,0.0420868345896532,
18.8241389928656));
#28226=CARTESIAN_POINT('Ctrl Pts',(1.85855788388951,2.93745562119467,18.9824313315753));
#28227=CARTESIAN_POINT('Ctrl Pts',(-1.45428025938601,3.15361087477854,19.1407236702849));
#28228=CARTESIAN_POINT('Ctrl Pts',(-2.76947321735942,1.39165108452637,19.2462518960914));
#28229=CARTESIAN_POINT('Ctrl Pts',(-2.91090525077877,0.426608275808834,
19.2990160089946));
#28230=CARTESIAN_POINT('Ctrl Pts',(1.59774743137964,-2.24059110187414,-0.219489327336925));
#28231=CARTESIAN_POINT('Ctrl Pts',(2.34056320305811,-1.71089517020912,-0.1667252144337));
#28232=CARTESIAN_POINT('Ctrl Pts',(3.24555696590951,0.135918132191012,-0.0611969886272476));
#28233=CARTESIAN_POINT('Ctrl Pts',(1.65137916205666,2.80087729111192,0.0970953500824295));
#28234=CARTESIAN_POINT('Ctrl Pts',(-1.44742355922437,2.90812226203881,0.255387688792107));
#28235=CARTESIAN_POINT('Ctrl Pts',(-3.22791977503548,0.372188659697663,
0.413680027501785));
#28236=CARTESIAN_POINT('Ctrl Pts',(-2.07045657173057,-2.50464714445445,
0.571972366211461));
#28237=CARTESIAN_POINT('Ctrl Pts',(0.971923218997645,-3.10042919965138,
0.73026470492114));
#28238=CARTESIAN_POINT('Ctrl Pts',(3.12946591806831,-0.874496900408864,
0.888557043630815));
#28239=CARTESIAN_POINT('Ctrl Pts',(2.43834241325956,2.14778225573103,1.0468493823405));
#28240=CARTESIAN_POINT('Ctrl Pts',(-0.472408462535135,3.2147991692499,1.20514172105017));
#28241=CARTESIAN_POINT('Ctrl Pts',(-2.95311556954223,1.35549938358592,1.36343405975985));
#28242=CARTESIAN_POINT('Ctrl Pts',(-2.7456392463286,-1.73774107914402,1.52172639846952));
#28243=CARTESIAN_POINT('Ctrl Pts',(-0.0388310450667128,-3.24911070164229,
1.68001873717921));
#28244=CARTESIAN_POINT('Ctrl Pts',(2.70332249559475,-1.80285945823596,1.83831107588888));
#28245=CARTESIAN_POINT('Ctrl Pts',(2.98466994900496,1.28452279209847,1.99660341459856));
#28246=CARTESIAN_POINT('Ctrl Pts',(0.549101832577521,3.20261363744452,2.15489575330824));
#28247=CARTESIAN_POINT('Ctrl Pts',(-2.38630783655485,2.20539926831328,2.31318809201791));
#28248=CARTESIAN_POINT('Ctrl Pts',(-3.1494856946562,-0.799368720665158,
2.47148043072759));
#28249=CARTESIAN_POINT('Ctrl Pts',(-1.04571838023061,-3.07647895214574,
2.62977276943727));
#28250=CARTESIAN_POINT('Ctrl Pts',(2.00995579213185,-2.55310164315028,2.78806510814695));
#28251=CARTESIAN_POINT('Ctrl Pts',(3.2359874868512,0.2943384893617,2.94635744685662));
#28252=CARTESIAN_POINT('Ctrl Pts',(1.51633237256273,2.87384519427829,3.1046497855663));
#28253=CARTESIAN_POINT('Ctrl Pts',(-1.58362481232089,2.83731961682751,3.26294212427598));
#28254=CARTESIAN_POINT('Ctrl Pts',(-3.24202429381481,0.218010568516082,
3.42123446298566));
#28255=CARTESIAN_POINT('Ctrl Pts',(-1.94924173227183,-2.59975129355074,
3.57952680169533));
#28256=CARTESIAN_POINT('Ctrl Pts',(1.11791593261785,-3.05098575865054,3.73781914040501));
#28257=CARTESIAN_POINT('Ctrl Pts',(3.16744599097691,-0.724938633091413,
3.89611147911469));
#28258=CARTESIAN_POINT('Ctrl Pts',(2.33368188527572,2.26101282279612,4.05440381782437));
#28259=CARTESIAN_POINT('Ctrl Pts',(-0.624409321422887,3.18878709348887,
4.21269615653404));
#28260=CARTESIAN_POINT('Ctrl Pts',(-3.01410701574777,1.21384060945571,4.37098849524372));
#28261=CARTESIAN_POINT('Ctrl Pts',(-2.66009347001759,-1.8660527479815,4.5292808339534));
#28262=CARTESIAN_POINT('Ctrl Pts',(0.115376352811499,-3.24729709526712,
4.68757317266307));
#28263=CARTESIAN_POINT('Ctrl Pts',(2.78582024445854,-1.6725596232017,4.84586551137275));
#28264=CARTESIAN_POINT('Ctrl Pts',(2.92036004329352,1.42469201764329,5.00415785008243));
#28265=CARTESIAN_POINT('Ctrl Pts',(0.396525526347995,3.22506087300498,5.16245018879211));
#28266=CARTESIAN_POINT('Ctrl Pts',(-2.48826218101693,2.08968931808907,5.32074252750178));
#28267=CARTESIAN_POINT('Ctrl Pts',(-3.10800990191072,-0.947905363019727,
5.47903486621146));
#28268=CARTESIAN_POINT('Ctrl Pts',(-0.898567531873009,-3.12263134524142,
5.63732720492114));
#28269=CARTESIAN_POINT('Ctrl Pts',(2.12883180659201,-2.45485748402225,5.79561954363082));
#28270=CARTESIAN_POINT('Ctrl Pts',(3.21837700605687,0.447548404647735,5.9539118823405));
#28271=CARTESIAN_POINT('Ctrl Pts',(1.37826605197434,2.94255549099653,6.11220422105017));
#28272=CARTESIAN_POINT('Ctrl Pts',(-1.71646659894271,2.75898396920541,6.27049655975985));
#28273=CARTESIAN_POINT('Ctrl Pts',(-3.24871700353266,0.063937145512284,
6.42878889846952));
#28274=CARTESIAN_POINT('Ctrl Pts',(-1.82369306064193,-2.68931101737694,
6.58708123717921));
#28275=CARTESIAN_POINT('Ctrl Pts',(1.26142029602366,-2.99450646424383,6.74537357588887));
#28276=CARTESIAN_POINT('Ctrl Pts',(3.1982754699156,-0.573832855590093,6.90366591459857));
#28277=CARTESIAN_POINT('Ctrl Pts',(2.22377271602456,2.36919501837296,7.06195825330823));
#28278=CARTESIAN_POINT('Ctrl Pts',(-0.775007929900716,3.15556854405185,
7.22025059201791));
#28279=CARTESIAN_POINT('Ctrl Pts',(-3.06830666783054,1.06945982615765,7.37854293072759));
#28280=CARTESIAN_POINT('Ctrl Pts',(-2.56855676867922,-1.99016739338446,
7.53683526943726));
#28281=CARTESIAN_POINT('Ctrl Pts',(0.269324470876077,-3.23816529179809,
7.69512760814696));
#28282=CARTESIAN_POINT('Ctrl Pts',(2.86204235886687,-1.53849395958199,7.85341994685661));
#28283=CARTESIAN_POINT('Ctrl Pts',(2.84947193147761,1.56165291897392,8.01171228556631));
#28284=CARTESIAN_POINT('Ctrl Pts',(0.243055922074948,3.24024288385343,8.17000462427597));
#28285=CARTESIAN_POINT('Ctrl Pts',(-2.5846114436551,1.96927240699339,8.32829696298566));
#28286=CARTESIAN_POINT('Ctrl Pts',(-3.059533060151,-1.0943068954647,8.48658930169534));
#28287=CARTESIAN_POINT('Ctrl Pts',(-0.749392566215293,-3.16174965949548,
8.64488164040499));
#28288=CARTESIAN_POINT('Ctrl Pts',(2.24291242830675,-2.35108357285861,8.8031739791147));
#28289=CARTESIAN_POINT('Ctrl Pts',(3.19351684359565,0.59975019573934,8.96146631782435));
#28290=CARTESIAN_POINT('Ctrl Pts',(1.23709506068279,3.00463740548719,9.11975865653406));
#28291=CARTESIAN_POINT('Ctrl Pts',(-1.84544188842464,2.67443346600101,9.27805099524372));
#28292=CARTESIAN_POINT('Ctrl Pts',(-3.24809168501307,-0.0902803044271455,
9.4363433339534));
#28293=CARTESIAN_POINT('Ctrl Pts',(-1.69403635526719,-2.77281282358755,
9.59463567266307));
#28294=CARTESIAN_POINT('Ctrl Pts',(1.40208319604178,-2.93128177407014,9.75292801137276));
#28295=CARTESIAN_POINT('Ctrl Pts',(3.22190054430279,-0.421434467313608,
9.91122035008243));
#28296=CARTESIAN_POINT('Ctrl Pts',(2.10885429766158,2.47204038778753,10.0695126887921));
#28297=CARTESIAN_POINT('Ctrl Pts',(-0.923860762935242,3.11524179131047,
10.2278050275018));
#28298=CARTESIAN_POINT('Ctrl Pts',(-3.1155946817763,0.922669987864471,10.3860973662115));
#28299=CARTESIAN_POINT('Ctrl Pts',(-2.47123416101382,-2.10979900679111,
10.5443897049211));
#28300=CARTESIAN_POINT('Ctrl Pts',(0.422665911219942,-3.2217392282913,10.7026820436308));
#28301=CARTESIAN_POINT('Ctrl Pts',(2.93181746413178,-1.40096269922882,10.8609743823405));
#28302=CARTESIAN_POINT('Ctrl Pts',(2.7721651265401,1.69509605592528,11.0192667210502));
#28303=CARTESIAN_POINT('Ctrl Pts',(0.0890388123653499,3.24812595468695,
11.1775590597599));
#28304=CARTESIAN_POINT('Ctrl Pts',(-2.67513863536514,1.84441953177557,11.3358513984695));
#28305=CARTESIAN_POINT('Ctrl Pts',(-3.00416434358826,-1.23824340270056,
11.4941437371792));
#28306=CARTESIAN_POINT('Ctrl Pts',(-0.598529526056383,-3.19374584681644,
11.6524360758889));
#28307=CARTESIAN_POINT('Ctrl Pts',(2.35194068701519,-2.24201363340657,11.8107284145986));
#28308=CARTESIAN_POINT('Ctrl Pts',(3.16146299574704,0.750600995296923,11.9690207533082));
#28309=CARTESIAN_POINT('Ctrl Pts',(1.0931374009324,3.05995110259973,12.1273130920179));
#28310=CARTESIAN_POINT('Ctrl Pts',(-1.97026015322306,2.58385855964291,12.2856054307276));
#28311=CARTESIAN_POINT('Ctrl Pts',(-3.24014974634217,-0.244294389819381,
12.4438977694372));
#28312=CARTESIAN_POINT('Ctrl Pts',(-1.56056367985961,-2.85006861824793,
12.602190108147));
#28313=CARTESIAN_POINT('Ctrl Pts',(1.53958777691108,-2.86145410670948,12.7604824468566));
#28314=CARTESIAN_POINT('Ctrl Pts',(3.23826799645081,-0.268086759801421,
12.9187747855663));
#28315=CARTESIAN_POINT('Ctrl Pts',(1.9891854943506,2.56931726275365,13.077067124276));
#28316=CARTESIAN_POINT('Ctrl Pts',(-1.07063251608334,3.06789767481307,13.2353594629857));
#28317=CARTESIAN_POINT('Ctrl Pts',(-3.15586453704825,0.773801752013446,
13.3936518016953));
#28318=CARTESIAN_POINT('Ctrl Pts',(-2.36834487499894,-2.22467810720716,
13.551944140405));
#28319=CARTESIAN_POINT('Ctrl Pts',(0.57505525838988,-3.19805590592392,13.7102364791147));
#28320=CARTESIAN_POINT('Ctrl Pts',(2.9949883855185,-1.26027564374785,13.8685288178244));
#28321=CARTESIAN_POINT('Ctrl Pts',(2.68861376905027,1.82472083577363,14.0268211565341));
#28322=CARTESIAN_POINT('Ctrl Pts',(-0.065178865321708,3.24869232817101,
14.1851134952437));
#28323=CARTESIAN_POINT('Ctrl Pts',(-2.75963983545724,1.71541193483002,14.3434058339534));
#28324=CARTESIAN_POINT('Ctrl Pts',(-2.94202847527452,-1.37939065474297,
14.5016981726631));
#28325=CARTESIAN_POINT('Ctrl Pts',(-0.446318244008518,-3.21854783288125,
14.6599905113728));
#28326=CARTESIAN_POINT('Ctrl Pts',(2.4556709866628,-2.12789335559991,14.8182828500824));
#28327=CARTESIAN_POINT('Ctrl Pts',(3.12228766678788,0.899760998324197,14.9765751887921));
#28328=CARTESIAN_POINT('Ctrl Pts',(0.946717350199806,3.10837198310357,15.1348675275018));
#28329=CARTESIAN_POINT('Ctrl Pts',(-2.09064022859603,2.48746327853901,15.2931598662115));
#28330=CARTESIAN_POINT('Ctrl Pts',(-3.22490907805967,-0.397758180478594,
15.4514522049212));
#28331=CARTESIAN_POINT('Ctrl Pts',(-1.42357569253155,-2.92090437480966,
15.6097445436308));
#28332=CARTESIAN_POINT('Ctrl Pts',(1.67362429492704,-2.78518075698867,15.7680368823405));
#28333=CARTESIAN_POINT('Ctrl Pts',(3.24734096140562,-0.114135159393468,
15.9263292210501));
#28334=CARTESIAN_POINT('Ctrl Pts',(1.86503586284711,2.66080651214107,16.0846215597599));
#28335=CARTESIAN_POINT('Ctrl Pts',(-1.21499255734613,3.01364285325432,16.2429138984695));
#28336=CARTESIAN_POINT('Ctrl Pts',(-3.18902555148107,0.623190435245776,
16.4012062371792));
#28337=CARTESIAN_POINT('Ctrl Pts',(-2.26012062205723,-2.33454587607517,
16.5594985758889));
#28338=CARTESIAN_POINT('Ctrl Pts',(0.726149134680179,-3.16716875562783,
16.7177909145985));
#28339=CARTESIAN_POINT('Ctrl Pts',(3.05141302899288,-1.11674954666312,16.8760832533082));
#28340=CARTESIAN_POINT('Ctrl Pts',(2.59900567611102,1.95023496759446,17.0343755920179));
#28341=CARTESIAN_POINT('Ctrl Pts',(-0.219248977230838,3.24194130019299,
17.1926679307276));
#28342=CARTESIAN_POINT('Ctrl Pts',(-2.83792611897795,1.58253912576034,17.3509602694372));
#28343=CARTESIAN_POINT('Ctrl Pts',(-2.87326270720222,-1.51742862006368,
17.509252608147));
#28344=CARTESIAN_POINT('Ctrl Pts',(-0.293106773496658,-3.23610372955733,
17.6675449468566));
#28345=CARTESIAN_POINT('Ctrl Pts',(2.55387956392575,-2.00897220462033,17.8258372855663));
#28346=CARTESIAN_POINT('Ctrl Pts',(3.07606020105273,1.04687969394011,17.984129624276));
#28347=CARTESIAN_POINT('Ctrl Pts',(0.798200826275583,3.14981869053862,18.1424219629856));
#28348=CARTESIAN_POINT('Ctrl Pts',(-2.20637986970829,2.38541183692082,18.3007143016953));
#28349=CARTESIAN_POINT('Ctrl Pts',(-3.20227239660768,-0.5502249209207,18.459006640405));
#28350=CARTESIAN_POINT('Ctrl Pts',(-1.28363234037996,-2.98535353825586,
18.6172989791147));
#28351=CARTESIAN_POINT('Ctrl Pts',(1.80437123226795,-2.70226477767009,18.7755913178244));
#28352=CARTESIAN_POINT('Ctrl Pts',(3.24817798824295,0.0393675940022248,
18.9338836565341));
#28353=CARTESIAN_POINT('Ctrl Pts',(1.73847600837534,2.74766590127781,19.0921759952437));
#28354=CARTESIAN_POINT('Ctrl Pts',(-1.36031885921439,2.94985531151743,19.2504683339534));
#28355=CARTESIAN_POINT('Ctrl Pts',(-2.59053688128428,1.30173617052782,19.3559965597598));
#28356=CARTESIAN_POINT('Ctrl Pts',(-2.72283095673202,0.399045011671049,
19.4087606726631));
#28357=CARTESIAN_POINT('Ctrl Pts',(1.48738611075532,-2.08582659521589,-0.109744663668464));
#28358=CARTESIAN_POINT('Ctrl Pts',(2.17889331642833,-1.5927183878681,-0.0569805507652379));
#28359=CARTESIAN_POINT('Ctrl Pts',(3.02137638149139,0.12652984949328,0.0485476750412134));
#28360=CARTESIAN_POINT('Ctrl Pts',(1.5373133331298,2.60741209712512,0.206840013750891));
#28361=CARTESIAN_POINT('Ctrl Pts',(-1.34744556998685,2.70724932863752,0.365132352460568));
#28362=CARTESIAN_POINT('Ctrl Pts',(-3.00495744554222,0.346480446247313,
0.523424691170246));
#28363=CARTESIAN_POINT('Ctrl Pts',(-1.92744377943072,-2.33164347620807,
0.681717029879923));
#28364=CARTESIAN_POINT('Ctrl Pts',(0.904789498180845,-2.88627303563221,
0.8400093685896));
#28365=CARTESIAN_POINT('Ctrl Pts',(2.91330409875712,-0.814092714543464,
0.998301707299278));
#28366=CARTESIAN_POINT('Ctrl Pts',(2.26991861637116,1.99942834102545,1.15659404600895));
#28367=CARTESIAN_POINT('Ctrl Pts',(-0.439777759599539,2.99274312028224,
1.31488638471863));
#28368=CARTESIAN_POINT('Ctrl Pts',(-2.74913481024945,1.26187087939309,1.47317872342831));
#28369=CARTESIAN_POINT('Ctrl Pts',(-2.55598951369148,-1.61770996744832,
1.63147106213799));
#28370=CARTESIAN_POINT('Ctrl Pts',(-0.0361488655615895,-3.02468464978613,
1.78976340084767));
#28371=CARTESIAN_POINT('Ctrl Pts',(2.51659571085528,-1.67833042016441,1.94805573955734));
#28372=CARTESIAN_POINT('Ctrl Pts',(2.77850963184176,1.19579685899802,2.10634807826702));
#28373=CARTESIAN_POINT('Ctrl Pts',(0.511173683102615,2.9813992805717,2.26464041697669));
#28374=CARTESIAN_POINT('Ctrl Pts',(-2.22147822764042,2.05306556964801,2.42293275568638));
#28375=CARTESIAN_POINT('Ctrl Pts',(-2.93194104790966,-0.744153868839558,
2.58122509439605));
#28376=CARTESIAN_POINT('Ctrl Pts',(-0.973487401055298,-2.86397710525587,
2.73951743310573));
#28377=CARTESIAN_POINT('Ctrl Pts',(1.87112197443351,-2.37675107390986,2.8978097718154));
#28378=CARTESIAN_POINT('Ctrl Pts',(3.01246789573266,0.274007626198644,3.05610211052509));
#28379=CARTESIAN_POINT('Ctrl Pts',(1.41159464001826,2.67533988318758,3.21439444923477));
#28380=CARTESIAN_POINT('Ctrl Pts',(-1.47423898435543,2.64133723951521,3.37268678794443));
#28381=CARTESIAN_POINT('Ctrl Pts',(-3.01808772190458,0.202951909194227,
3.53097912665412));
#28382=CARTESIAN_POINT('Ctrl Pts',(-1.81460162109742,-2.4201784897295,3.68927146536379));
#28383=CARTESIAN_POINT('Ctrl Pts',(1.04069804683216,-2.84024480490672,3.84756380407347));
#28384=CARTESIAN_POINT('Ctrl Pts',(2.94866077142029,-0.674864895936037,
4.00585614278315));
#28385=CARTESIAN_POINT('Ctrl Pts',(2.17248731239275,2.10483772517333,4.16414848149283));
#28386=CARTESIAN_POINT('Ctrl Pts',(-0.581279452478057,2.96852777845849,
4.3224408202025));
#28387=CARTESIAN_POINT('Ctrl Pts',(-2.80591339000449,1.12999691172477,4.48073315891218));
#28388=CARTESIAN_POINT('Ctrl Pts',(-2.47635264680012,-1.73715875536589,
4.63902549762186));
#28389=CARTESIAN_POINT('Ctrl Pts',(0.107406953884614,-3.02299631477157,
4.79731783633154));
#28390=CARTESIAN_POINT('Ctrl Pts',(2.5933950869135,-1.55703079479352,4.95561017504121));
#28391=CARTESIAN_POINT('Ctrl Pts',(2.71864180876751,1.32628416577508,5.1139025137509));
#28392=CARTESIAN_POINT('Ctrl Pts',(0.369136290797007,3.0022960166526,5.27219485246056));
#28393=CARTESIAN_POINT('Ctrl Pts',(-2.31639027250168,1.94534806094824,5.43048719117025));
#28394=CARTESIAN_POINT('Ctrl Pts',(-2.89333011551159,-0.88243062925697,
5.58877952987992));
#28395=CARTESIAN_POINT('Ctrl Pts',(-0.836500713588696,-2.90694161085946,
5.7470718685896));
#28396=CARTESIAN_POINT('Ctrl Pts',(1.98178685759173,-2.28529294049032,5.90536420729928));
#28397=CARTESIAN_POINT('Ctrl Pts',(2.99607382491597,0.416634862237868,6.06365654600896));
#28398=CARTESIAN_POINT('Ctrl Pts',(1.28306498409578,2.73930414875135,6.22194888471863));
#28399=CARTESIAN_POINT('Ctrl Pts',(-1.59790498091322,2.56841247558709,6.38024122342832));
#28400=CARTESIAN_POINT('Ctrl Pts',(-3.0243181456137,0.0595208105665224,
6.53853356213798));
#28401=CARTESIAN_POINT('Ctrl Pts',(-1.69772498168712,-2.50355204845721,
6.69682590084767));
#28402=CARTESIAN_POINT('Ctrl Pts',(1.17429012325833,-2.78766670877218,6.85511823955734));
#28403=CARTESIAN_POINT('Ctrl Pts',(2.97736076359342,-0.534196458424437,
7.01341057826702));
#28404=CARTESIAN_POINT('Ctrl Pts',(2.07016990691417,2.20554744435157,7.1717029169767));
#28405=CARTESIAN_POINT('Ctrl Pts',(-0.721475752687772,2.93760373622148,
7.32999525568637));
#28406=CARTESIAN_POINT('Ctrl Pts',(-2.85636930570956,0.995588952419164,
7.48828759439606));
#28407=CARTESIAN_POINT('Ctrl Pts',(-2.39113866646689,-1.85270042114361,
7.64657993310571));
#28408=CARTESIAN_POINT('Ctrl Pts',(0.250721402769973,-3.01449527300539,
7.80487227181542));
#28409=CARTESIAN_POINT('Ctrl Pts',(2.66435230585608,-1.43222545817973,7.96316461052508));
#28410=CARTESIAN_POINT('Ctrl Pts',(2.65265015648138,1.45378475714189,8.12145694923476));
#28411=CARTESIAN_POINT('Ctrl Pts',(0.226267303286426,3.01642935939867,8.27974928794444));
#28412=CARTESIAN_POINT('Ctrl Pts',(-2.4060843957498,1.83324871561609,8.43804162665412));
#28413=CARTESIAN_POINT('Ctrl Pts',(-2.8482017180499,-1.01871975836163,8.59633396536379));
#28414=CARTESIAN_POINT('Ctrl Pts',(-0.697629720818526,-2.94335790304364,
8.75462630407348));
#28415=CARTESIAN_POINT('Ctrl Pts',(2.0879875805047,-2.18868701198616,8.91291864278314));
#28416=CARTESIAN_POINT('Ctrl Pts',(2.97293083020372,0.558323608315999,9.07121098149283));
#28417=CARTESIAN_POINT('Ctrl Pts',(1.15164510660782,2.797097874799,9.2295033202025));
#28418=CARTESIAN_POINT('Ctrl Pts',(-1.71797155115982,2.4897021352331,9.38779565891218));
#28419=CARTESIAN_POINT('Ctrl Pts',(-3.02373601976415,-0.0840443666141708,
9.54608799762186));
#28420=CARTESIAN_POINT('Ctrl Pts',(-1.57702406303557,-2.58128612853855,
9.70438033633154));
#28421=CARTESIAN_POINT('Ctrl Pts',(1.3052370048971,-2.72880914206656,9.86267267504121));
#28422=CARTESIAN_POINT('Ctrl Pts',(2.99935398155699,-0.392324694732591,
10.0209650137509));
#28423=CARTESIAN_POINT('Ctrl Pts',(1.96318925653975,2.30128896833614,10.1792573524606));
#28424=CARTESIAN_POINT('Ctrl Pts',(-0.860046863524081,2.90006247610654,
10.3375496911703));
#28425=CARTESIAN_POINT('Ctrl Pts',(-2.90039099134443,0.858938338943435,
10.4958420298799));
#28426=CARTESIAN_POINT('Ctrl Pts',(-2.30053843012103,-1.9640687117092,10.6541343685896));
#28427=CARTESIAN_POINT('Ctrl Pts',(0.393471079027465,-2.9992038081377,10.8124267072993));
#28428=CARTESIAN_POINT('Ctrl Pts',(2.72930783037093,-1.30419390423922,10.970719046009));
#28429=CARTESIAN_POINT('Ctrl Pts',(2.58068316991478,1.57801056691565,11.1290113847186));
#28430=CARTESIAN_POINT('Ctrl Pts',(0.0828886282207864,3.02376792232645,
11.2873037234283));
#28431=CARTESIAN_POINT('Ctrl Pts',(-2.4903585963842,1.7170198118234,11.445596062138));
#28432=CARTESIAN_POINT('Ctrl Pts',(-2.79665748873786,-1.15271412911671,
11.6038884008477));
#28433=CARTESIAN_POINT('Ctrl Pts',(-0.557187254035818,-2.97314401546895,
11.7621807395573));
#28434=CARTESIAN_POINT('Ctrl Pts',(2.18948492263639,-2.08715086812781,11.920473078267));
#28435=CARTESIAN_POINT('Ctrl Pts',(2.94309104004043,0.698754679993293,12.0787654169767));
#28436=CARTESIAN_POINT('Ctrl Pts',(1.01763104440733,2.8485908850232,12.2370577556864));
#28437=CARTESIAN_POINT('Ctrl Pts',(-1.83416823518104,2.40538351574787,12.3953500943961));
#28438=CARTESIAN_POINT('Ctrl Pts',(-3.01634265518126,-0.227420226261331,
12.5536424331057));
#28439=CARTESIAN_POINT('Ctrl Pts',(-1.45277075511745,-2.65320562826448,
12.7119347718154));
#28440=CARTESIAN_POINT('Ctrl Pts',(1.43324372218759,-2.6638046860813,12.8702271105251));
#28441=CARTESIAN_POINT('Ctrl Pts',(3.01459088353241,-0.249569184199341,
13.0285194492348));
#28442=CARTESIAN_POINT('Ctrl Pts',(1.8517863448907,2.39184663088069,13.1868117879444));
#28443=CARTESIAN_POINT('Ctrl Pts',(-0.996680641051226,2.85598856309551,
13.3451041266541));
#28444=CARTESIAN_POINT('Ctrl Pts',(-2.93787928407284,0.720352889210458,
13.5033964653638));
#28445=CARTESIAN_POINT('Ctrl Pts',(-2.20475602299055,-2.071012759948,13.6616888040735));
#28446=CARTESIAN_POINT('Ctrl Pts',(0.535334426109747,-2.97715636556076,
13.8199811427831));
#28447=CARTESIAN_POINT('Ctrl Pts',(2.78811534226478,-1.17322453562959,13.9782734814928));
#28448=CARTESIAN_POINT('Ctrl Pts',(2.50290296121319,1.69868176523493,14.1365658202025));
#28449=CARTESIAN_POINT('Ctrl Pts',(-0.0606767609763033,3.02429517465504,
14.2948581589122));
#28450=CARTESIAN_POINT('Ctrl Pts',(-2.56902303914322,1.59692316568888,14.4531504976219));
#28451=CARTESIAN_POINT('Ctrl Pts',(-2.73881353562333,-1.28411190709835,
14.6114428363315));
#28452=CARTESIAN_POINT('Ctrl Pts',(-0.415489672570913,-2.99623285220711,
14.7697351750412));
#28453=CARTESIAN_POINT('Ctrl Pts',(2.28605025200581,-1.98091322829095,14.9280275137509));
#28454=CARTESIAN_POINT('Ctrl Pts',(2.90662167133189,0.837611743647851,15.0863198524606));
#28455=CARTESIAN_POINT('Ctrl Pts',(0.881324676130029,2.89366718664477,15.2446121911703));
#28456=CARTESIAN_POINT('Ctrl Pts',(-1.94623328914695,2.31564655267074,15.4029045298799));
#28457=CARTESIAN_POINT('Ctrl Pts',(-3.00215470665022,-0.370283801722237,
15.5611968685896));
#28458=CARTESIAN_POINT('Ctrl Pts',(-1.32524494866622,-2.71914854163458,
15.7194892072993));
#28459=CARTESIAN_POINT('Ctrl Pts',(1.55802192637397,-2.59279977080658,15.877781546009));
#28460=CARTESIAN_POINT('Ctrl Pts',(3.0230371509412,-0.106251493506751,16.0360738847186));
#28461=CARTESIAN_POINT('Ctrl Pts',(1.73621210960984,2.47701643691491,16.1943662234283));
#28462=CARTESIAN_POINT('Ctrl Pts',(-1.13106929103762,2.80548128863956,16.352658562138));
#28463=CARTESIAN_POINT('Ctrl Pts',(-2.96874976542504,0.580144758511495,
16.5109509008477));
#28464=CARTESIAN_POINT('Ctrl Pts',(-2.10400715147876,-2.173291624695,16.6692432395573));
#28465=CARTESIAN_POINT('Ctrl Pts',(0.675991784463513,-2.94840268556796,
16.827535578267));
#28466=CARTESIAN_POINT('Ctrl Pts',(2.84064256237469,-1.03961222673644,16.9858279169767));
#28467=CARTESIAN_POINT('Ctrl Pts',(2.41948437437558,1.81552625060683,17.1441202556864));
#28468=CARTESIAN_POINT('Ctrl Pts',(-0.204104777216815,3.01801046090703,
17.3024125943961));
#28469=CARTESIAN_POINT('Ctrl Pts',(-2.64190184870001,1.47322828949895,17.4607049331057));
#28470=CARTESIAN_POINT('Ctrl Pts',(-2.67479763028224,-1.41261516633856,
17.6189972718154));
#28471=CARTESIAN_POINT('Ctrl Pts',(-0.272860988730089,-3.01257610919817,
17.7772896105251));
#28472=CARTESIAN_POINT('Ctrl Pts',(2.37747526130895,-1.87020632633128,17.9355819492348));
#28473=CARTESIAN_POINT('Ctrl Pts',(2.86358727858653,0.974568499261341,18.0938742879444));
#28474=CARTESIAN_POINT('Ctrl Pts',(0.74306664450121,2.93225104274409,18.2521666266541));
#28475=CARTESIAN_POINT('Ctrl Pts',(-2.05397843789397,2.22064411745206,18.4104589653638));
#28476=CARTESIAN_POINT('Ctrl Pts',(-2.98108161028717,-0.512219196285761,
18.5687513040735));
#28477=CARTESIAN_POINT('Ctrl Pts',(-1.19496791351362,-2.77914600348429,
18.7270436427832));
#28478=CARTESIAN_POINT('Ctrl Pts',(1.67973777132246,-2.51561105275516,18.8853359814928));
#28479=CARTESIAN_POINT('Ctrl Pts',(3.02381636176497,0.0366483534147998,
19.0436283202025));
#28480=CARTESIAN_POINT('Ctrl Pts',(1.61839413286117,2.55787618136095,19.2019206589122));
#28481=CARTESIAN_POINT('Ctrl Pts',(-1.26635745904276,2.74609974825633,19.3602129976219));
#28482=CARTESIAN_POINT('Ctrl Pts',(-2.41160054520915,1.21182125652926,19.4657412234283));
#28483=CARTESIAN_POINT('Ctrl Pts',(-2.53475666268528,0.371481747533264,
19.5185053363315));
#28484=CARTESIAN_POINT('Ctrl Pts',(1.37702479013101,-1.93106208855765,-2.4980018054066E-15));
#28485=CARTESIAN_POINT('Ctrl Pts',(2.01722342979855,-1.47454160552709,0.0527641129032233));
#28486=CARTESIAN_POINT('Ctrl Pts',(2.79719579707326,0.117141566795549,0.158292338709675));
#28487=CARTESIAN_POINT('Ctrl Pts',(1.42324750420295,2.41394690313832,0.316584677419352));
#28488=CARTESIAN_POINT('Ctrl Pts',(-1.24746758074934,2.50637639523624,0.474877016129029));
#28489=CARTESIAN_POINT('Ctrl Pts',(-2.78199511604896,0.320772232796965,
0.633169354838707));
#28490=CARTESIAN_POINT('Ctrl Pts',(-1.78443098713088,-2.15863980796169,
0.791461693548384));
#28491=CARTESIAN_POINT('Ctrl Pts',(0.837655777364047,-2.67211687161305,
0.949754032258061));
#28492=CARTESIAN_POINT('Ctrl Pts',(2.69714227944592,-0.753688528678065,
1.10804637096774));
#28493=CARTESIAN_POINT('Ctrl Pts',(2.10149481948277,1.85107442631988,1.26633870967742));
#28494=CARTESIAN_POINT('Ctrl Pts',(-0.407147056663944,2.77068707131458,
1.42463104838709));
#28495=CARTESIAN_POINT('Ctrl Pts',(-2.54515405095666,1.16824237520026,1.58292338709677));
#28496=CARTESIAN_POINT('Ctrl Pts',(-2.36633978105435,-1.49767885575262,
1.74121572580645));
#28497=CARTESIAN_POINT('Ctrl Pts',(-0.0334666860564693,-2.80025859792997,
1.89950806451613));
#28498=CARTESIAN_POINT('Ctrl Pts',(2.32986892611582,-1.55380138209287,2.0578004032258));
#28499=CARTESIAN_POINT('Ctrl Pts',(2.57234931467855,1.10707092589757,2.21609274193548));
#28500=CARTESIAN_POINT('Ctrl Pts',(0.473245533627712,2.76018492369889,2.37438508064516));
#28501=CARTESIAN_POINT('Ctrl Pts',(-2.05664861872599,1.90073187098275,2.53267741935483));
#28502=CARTESIAN_POINT('Ctrl Pts',(-2.71439640116312,-0.688939017013961,
2.69096975806451));
#28503=CARTESIAN_POINT('Ctrl Pts',(-0.901256421879981,-2.65147525836599,
2.84926209677419));
#28504=CARTESIAN_POINT('Ctrl Pts',(1.73228815673516,-2.20040050466946,3.00755443548387));
#28505=CARTESIAN_POINT('Ctrl Pts',(2.78894830461411,0.253676763035589,3.16584677419355));
#28506=CARTESIAN_POINT('Ctrl Pts',(1.30685690747379,2.47683457209687,3.32413911290322));
#28507=CARTESIAN_POINT('Ctrl Pts',(-1.36485315638996,2.44535486220292,3.4824314516129));
#28508=CARTESIAN_POINT('Ctrl Pts',(-2.79415114999435,0.187893249872369,
3.64072379032258));
#28509=CARTESIAN_POINT('Ctrl Pts',(-1.67996150992302,-2.24060568590825,
3.79901612903226));
#28510=CARTESIAN_POINT('Ctrl Pts',(0.963480161046465,-2.62950385116291,
3.95730846774193));
#28511=CARTESIAN_POINT('Ctrl Pts',(2.72987555186367,-0.62479115878066,4.11560080645161));
#28512=CARTESIAN_POINT('Ctrl Pts',(2.01129273950979,1.94866262755053,4.27389314516129));
#28513=CARTESIAN_POINT('Ctrl Pts',(-0.538149583533225,2.74826846342811,
4.43218548387097));
#28514=CARTESIAN_POINT('Ctrl Pts',(-2.5977197642612,1.04615321399383,4.59047782258064));
#28515=CARTESIAN_POINT('Ctrl Pts',(-2.29261182358265,-1.60826476275027,
4.74877016129032));
#28516=CARTESIAN_POINT('Ctrl Pts',(0.099437554957728,-2.79869553427603,
4.9070625));
#28517=CARTESIAN_POINT('Ctrl Pts',(2.40096992936847,-1.44150196638533,5.06535483870968));
#28518=CARTESIAN_POINT('Ctrl Pts',(2.51692357424149,1.22787631390688,5.22364717741935));
#28519=CARTESIAN_POINT('Ctrl Pts',(0.341747055246021,2.77953116030023,5.38193951612902));
#28520=CARTESIAN_POINT('Ctrl Pts',(-2.14451836398642,1.80100680380742,5.54023185483871));
#28521=CARTESIAN_POINT('Ctrl Pts',(-2.67865032911246,-0.816955895494213,
5.69852419354838));
#28522=CARTESIAN_POINT('Ctrl Pts',(-0.774433895304387,-2.6912518764775,
5.85681653225807));
#28523=CARTESIAN_POINT('Ctrl Pts',(1.83474190859146,-2.11572839695838,6.01510887096773));
#28524=CARTESIAN_POINT('Ctrl Pts',(2.77377064377508,0.385721319828002,6.17340120967742));
#28525=CARTESIAN_POINT('Ctrl Pts',(1.18786391621721,2.53605280650616,6.3316935483871));
#28526=CARTESIAN_POINT('Ctrl Pts',(-1.47934336288373,2.37784098196877,6.48998588709676));
#28527=CARTESIAN_POINT('Ctrl Pts',(-2.79991928769473,0.0551044756207588,
6.64827822580646));
#28528=CARTESIAN_POINT('Ctrl Pts',(-1.57175690273231,-2.31779307953747,
6.80657056451611));
#28529=CARTESIAN_POINT('Ctrl Pts',(1.087159950493,-2.58082695330052,6.96486290322581));
#28530=CARTESIAN_POINT('Ctrl Pts',(2.75644605727123,-0.494560061258782,
7.12315524193547));
#28531=CARTESIAN_POINT('Ctrl Pts',(1.91656709780378,2.04189987033018,7.28144758064516));
#28532=CARTESIAN_POINT('Ctrl Pts',(-0.667943575474826,2.7196389283911,7.43973991935484));
#28533=CARTESIAN_POINT('Ctrl Pts',(-2.64443194358857,0.921718078680678,
7.59803225806451));
#28534=CARTESIAN_POINT('Ctrl Pts',(-2.21372056425457,-1.71523344890277,
7.75632459677419));
#28535=CARTESIAN_POINT('Ctrl Pts',(0.23211833466387,-2.79082525421268,7.91461693548387));
#28536=CARTESIAN_POINT('Ctrl Pts',(2.4666622528453,-1.32595695677747,8.07290927419355));
#28537=CARTESIAN_POINT('Ctrl Pts',(2.45582838148514,1.34591659530986,8.23120161290321));
#28538=CARTESIAN_POINT('Ctrl Pts',(0.209478684497901,2.79261583494391,8.38949395161291));
#28539=CARTESIAN_POINT('Ctrl Pts',(-2.22755734784449,1.6972250242388,8.54778629032258));
#28540=CARTESIAN_POINT('Ctrl Pts',(-2.6368703759488,-0.943132621258565,
8.70607862903226));
#28541=CARTESIAN_POINT('Ctrl Pts',(-0.645866875421753,-2.72496614659181,
8.86437096774193));
#28542=CARTESIAN_POINT('Ctrl Pts',(1.93306273270264,-2.02629045111372,9.02266330645161));
#28543=CARTESIAN_POINT('Ctrl Pts',(2.75234481681179,0.516897020892659,9.18095564516129));
#28544=CARTESIAN_POINT('Ctrl Pts',(1.06619515253284,2.58955834411081,9.33924798387097));
#28545=CARTESIAN_POINT('Ctrl Pts',(-1.590501213895,2.3049708044652,9.49754032258064));
#28546=CARTESIAN_POINT('Ctrl Pts',(-2.79938035451524,-0.077808428801199,
9.65583266129033));
#28547=CARTESIAN_POINT('Ctrl Pts',(-1.46001177080394,-2.38975943348956,
9.81412499999998));
#28548=CARTESIAN_POINT('Ctrl Pts',(1.20839081375242,-2.52633651006299,9.97241733870969));
#28549=CARTESIAN_POINT('Ctrl Pts',(2.77680741881119,-0.363214922151578,
10.1307096774193));
#28550=CARTESIAN_POINT('Ctrl Pts',(1.81752421541791,2.13053754888476,10.2890020161291));
#28551=CARTESIAN_POINT('Ctrl Pts',(-0.796232964112916,2.68488316090261,
10.4472943548387));
#28552=CARTESIAN_POINT('Ctrl Pts',(-2.68518730091256,0.795206690022401,
10.6055866935484));
#28553=CARTESIAN_POINT('Ctrl Pts',(-2.12984269922823,-1.81833841662728,
10.7638790322581));
#28554=CARTESIAN_POINT('Ctrl Pts',(0.364276246834986,-2.77666838798409,
10.9221713709677));
#28555=CARTESIAN_POINT('Ctrl Pts',(2.52679819661009,-1.20742510924963,11.0804637096774));
#28556=CARTESIAN_POINT('Ctrl Pts',(2.38920121328945,1.46092507790601,11.2387560483871));
#28557=CARTESIAN_POINT('Ctrl Pts',(0.0767384440762257,2.79940988996594,
11.3970483870968));
#28558=CARTESIAN_POINT('Ctrl Pts',(-2.30557855740325,1.58962009187123,11.5553407258065));
#28559=CARTESIAN_POINT('Ctrl Pts',(-2.58915063388745,-1.06718485553286,
11.7136330645161));
#28560=CARTESIAN_POINT('Ctrl Pts',(-0.515844982015253,-2.75254218412146,
11.8719254032258));
#28561=CARTESIAN_POINT('Ctrl Pts',(2.02702915825758,-1.93228810284904,12.0302177419355));
#28562=CARTESIAN_POINT('Ctrl Pts',(2.72471908433383,0.646908364689661,12.1885100806452));
#28563=CARTESIAN_POINT('Ctrl Pts',(0.942124687882267,2.63723066744667,12.3468024193548));
#28564=CARTESIAN_POINT('Ctrl Pts',(-1.69807631713903,2.22690847185283,12.5050947580645));
#28565=CARTESIAN_POINT('Ctrl Pts',(-2.79253556402036,-0.210546062703279,
12.6633870967742));
#28566=CARTESIAN_POINT('Ctrl Pts',(-1.3449778303753,-2.45634263828104,12.8216794354839));
#28567=CARTESIAN_POINT('Ctrl Pts',(1.3268996674641,-2.46615526545311,12.9799717741935));
#28568=CARTESIAN_POINT('Ctrl Pts',(2.79091377061401,-0.231051608597259,
13.1382641129033));
#28569=CARTESIAN_POINT('Ctrl Pts',(1.71438719543081,2.21437599900773,13.2965564516129));
#28570=CARTESIAN_POINT('Ctrl Pts',(-0.922728766019108,2.64407945137796,
13.4548487903226));
#28571=CARTESIAN_POINT('Ctrl Pts',(-2.71989403109743,0.666904026407466,
13.6131411290322));
#28572=CARTESIAN_POINT('Ctrl Pts',(-2.04116717098217,-1.91734741268884,
13.7714334677419));
#28573=CARTESIAN_POINT('Ctrl Pts',(0.495613593829615,-2.7562568251976,13.9297258064516));
#28574=CARTESIAN_POINT('Ctrl Pts',(2.58124229901106,-1.08617342751133,14.0880181451613));
#28575=CARTESIAN_POINT('Ctrl Pts',(2.31719215337611,1.57264269469624,14.246310483871));
#28576=CARTESIAN_POINT('Ctrl Pts',(-0.0561746566308962,2.79989802113906,
14.4046028225806));
#28577=CARTESIAN_POINT('Ctrl Pts',(-2.37840624282921,1.47843439654775,14.5628951612903));
#28578=CARTESIAN_POINT('Ctrl Pts',(-2.53559859597213,-1.18883315945374,
14.7211875));
#28579=CARTESIAN_POINT('Ctrl Pts',(-0.384661101133316,-2.77391787153297,
14.8794798387097));
#28580=CARTESIAN_POINT('Ctrl Pts',(2.11642951734883,-1.833933100982,15.0377721774193));
#28581=CARTESIAN_POINT('Ctrl Pts',(2.69095567587589,0.775462488971503,15.196064516129));
#28582=CARTESIAN_POINT('Ctrl Pts',(0.815932002060255,2.67896239018596,15.3543568548387));
#28583=CARTESIAN_POINT('Ctrl Pts',(-1.80182634969786,2.14382982680247,15.5126491935484));
#28584=CARTESIAN_POINT('Ctrl Pts',(-2.77940033524077,-0.342809422965879,
15.6709415322581));
#28585=CARTESIAN_POINT('Ctrl Pts',(-1.22691420480089,-2.5173927084595,15.8292338709677));
#28586=CARTESIAN_POINT('Ctrl Pts',(1.44241955782089,-2.40041878462448,15.9875262096774));
#28587=CARTESIAN_POINT('Ctrl Pts',(2.7987333404768,-0.0983678276200387,
16.1458185483871));
#28588=CARTESIAN_POINT('Ctrl Pts',(1.60738835637255,2.29322636168875,16.3041108870968));
#28589=CARTESIAN_POINT('Ctrl Pts',(-1.0471460247291,2.59731972402479,16.4624032258064));
#28590=CARTESIAN_POINT('Ctrl Pts',(-2.74847397936901,0.537099081777219,
16.6206955645161));
#28591=CARTESIAN_POINT('Ctrl Pts',(-1.94789368090028,-2.01203737331484,
16.7789879032258));
#28592=CARTESIAN_POINT('Ctrl Pts',(0.625834434246847,-2.72963661550809,
16.9372802419355));
#28593=CARTESIAN_POINT('Ctrl Pts',(2.62987209575649,-0.962474906809746,
17.0955725806452));
#28594=CARTESIAN_POINT('Ctrl Pts',(2.23996307264014,1.6808175336192,17.2538649193548));
#28595=CARTESIAN_POINT('Ctrl Pts',(-0.188960577202794,2.79407962162107,
17.4121572580645));
#28596=CARTESIAN_POINT('Ctrl Pts',(-2.44587757842207,1.36391745323756,17.5704495967742));
#28597=CARTESIAN_POINT('Ctrl Pts',(-2.47633255336226,-1.30780171261343,
17.7287419354839));
#28598=CARTESIAN_POINT('Ctrl Pts',(-0.252615203963521,-2.78904848883903,
17.8870342741935));
#28599=CARTESIAN_POINT('Ctrl Pts',(2.20107095869216,-1.73144044804223,18.0453266129032));
#28600=CARTESIAN_POINT('Ctrl Pts',(2.65111435612032,0.902257304582571,18.2036189516129));
#28601=CARTESIAN_POINT('Ctrl Pts',(0.687932462726838,2.71468339494958,18.3619112903226));
#28602=CARTESIAN_POINT('Ctrl Pts',(-1.90157700607965,2.0558763979833,18.5202036290323));
#28603=CARTESIAN_POINT('Ctrl Pts',(-2.75989082396666,-0.474213471650817,
18.6784959677419));
#28604=CARTESIAN_POINT('Ctrl Pts',(-1.10630348664728,-2.57293846871273,
18.8367883064516));
#28605=CARTESIAN_POINT('Ctrl Pts',(1.55510431037697,-2.32895732784023,18.9950806451613));
#28606=CARTESIAN_POINT('Ctrl Pts',(2.799454735287,0.0339291128273711,19.153372983871));
#28607=CARTESIAN_POINT('Ctrl Pts',(1.49831225734699,2.36808646144409,19.3116653225806));
#28608=CARTESIAN_POINT('Ctrl Pts',(-1.17239605887113,2.54234418499522,19.4699576612903));
#28609=CARTESIAN_POINT('Ctrl Pts',(-2.23266420913401,1.1219063425307,19.5754858870968));
#28610=CARTESIAN_POINT('Ctrl Pts',(-2.34668236863853,0.34391848339548,19.62825));
#28611=CARTESIAN_POINT('',(1.37702479013102,-1.93106208855765,0.));
#28612=CARTESIAN_POINT('Ctrl Pts',(1.37702479013101,-1.93106208855765,-2.4980018054066E-15));
#28613=CARTESIAN_POINT('Ctrl Pts',(2.01722342979855,-1.47454160552709,0.0527641129032233));
#28614=CARTESIAN_POINT('Ctrl Pts',(2.79719579707326,0.117141566795549,0.158292338709675));
#28615=CARTESIAN_POINT('Ctrl Pts',(1.42324750420295,2.41394690313832,0.316584677419352));
#28616=CARTESIAN_POINT('Ctrl Pts',(-1.24746758074934,2.50637639523624,0.474877016129029));
#28617=CARTESIAN_POINT('Ctrl Pts',(-2.32942948970535,0.965354551432513,
0.586485493020905));
#28618=CARTESIAN_POINT('Ctrl Pts',(-2.3750014795357,0.091963591913039,0.645329857009555));
#28619=CARTESIAN_POINT('Ctrl Pts',(-2.37433784198147,0.00164420209662409,
0.651410108094979));
#28620=CARTESIAN_POINT('Ctrl Pts',(1.29201086331817,2.64828936846223,6.41847686111419E-17));
#28621=CARTESIAN_POINT('Ctrl Pts',(1.35862032458796,2.60817485458433,2.61969259968471E-17));
#28622=CARTESIAN_POINT('Ctrl Pts',(1.42341581930837,2.56531698465799,3.28157858661721E-16));
#28623=CARTESIAN_POINT('Ctrl Pts',(1.48620178418383,2.51970672695701,2.04697370165263E-16));
#28624=CARTESIAN_POINT('Ctrl Pts',(1.56531098107701,2.46223861503148,5.43435251614495E-17));
#28625=CARTESIAN_POINT('Ctrl Pts',(1.64123143087454,2.40040132841406,-5.27955452558019E-16));
#28626=CARTESIAN_POINT('Ctrl Pts',(1.71378595850393,2.33457408786609,-7.3899220076612E-16));
#28627=CARTESIAN_POINT('Ctrl Pts',(1.75212006782637,2.29979433368659,-8.50493247512412E-16));
#28628=CARTESIAN_POINT('Ctrl Pts',(1.78951386694703,2.26390023027539,-3.7350885354349E-16));
#28629=CARTESIAN_POINT('Ctrl Pts',(1.82593618288559,2.22694486783177,-3.67761376907083E-16));
#28630=CARTESIAN_POINT('Ctrl Pts',(1.84259085550132,2.21004645137928,-3.65133253481123E-16));
#28631=CARTESIAN_POINT('Ctrl Pts',(1.85904234863816,2.19292611311178,-2.46595166079732E-16));
#28632=CARTESIAN_POINT('Ctrl Pts',(1.87528742149878,2.17558883786553,-2.63677968348475E-16));
#28633=CARTESIAN_POINT('Ctrl Pts',(1.88718261793227,2.16289389359258,-2.76186578827762E-16));
#28634=CARTESIAN_POINT('Ctrl Pts',(1.89896688194925,2.15008278084551,-1.10225564131519E-15));
#28635=CARTESIAN_POINT('Ctrl Pts',(1.91062984003561,2.13716785713421,-1.06165076729781E-15));
#28636=CARTESIAN_POINT('Ctrl Pts',(1.97578401617971,2.0650196758458,-8.34814908466034E-16));
#28637=CARTESIAN_POINT('Ctrl Pts',(2.03723207640777,1.98955383080639,-9.74476180451947E-16));
#28638=CARTESIAN_POINT('Ctrl Pts',(2.09480296364938,1.91114695058468,-8.46545056276682E-16));
#28639=CARTESIAN_POINT('Ctrl Pts',(2.142269300225,1.84650164903097,-7.41067755343023E-16));
#28640=CARTESIAN_POINT('Ctrl Pts',(2.1870993303121,1.77985624721179,2.24451139630718E-16));
#28641=CARTESIAN_POINT('Ctrl Pts',(2.229172411834,1.71141200033172,1.52655665885959E-16));
#28642=CARTESIAN_POINT('Ctrl Pts',(2.24800974392323,1.68076753690192,1.20510761531148E-16));
#28643=CARTESIAN_POINT('Ctrl Pts',(2.26629410220438,1.6497623951442,5.54871798735934E-17));
#28644=CARTESIAN_POINT('Ctrl Pts',(2.28401308817003,1.61841438574687,8.32667268468867E-17));
#28645=CARTESIAN_POINT('Ctrl Pts',(2.29435495135519,1.60011780687136,9.94805369769141E-17));
#28646=CARTESIAN_POINT('Ctrl Pts',(2.3045041967679,1.58170442532538,5.28474538527533E-16));
#28647=CARTESIAN_POINT('Ctrl Pts',(2.31445819927483,1.56317777718625,5.55111512312578E-16));
#28648=CARTESIAN_POINT('Ctrl Pts',(2.32185832866684,1.54940446405576,5.74914305458692E-16));
#28649=CARTESIAN_POINT('Ctrl Pts',(2.32915061183048,1.5355682586848,6.28531276475973E-16));
#28650=CARTESIAN_POINT('Ctrl Pts',(2.33632722813254,1.52168406757476,6.10622663543836E-16));
#28651=CARTESIAN_POINT('Ctrl Pts',(2.37998634723912,1.43721925465201,5.01675182986223E-16));
#28652=CARTESIAN_POINT('Ctrl Pts',(2.4194343086838,1.35085952195958,-2.85148112393472E-16));
#28653=CARTESIAN_POINT('Ctrl Pts',(2.45450882946931,1.26295234700174,-2.91433543964104E-16));
#28654=CARTESIAN_POINT('Ctrl Pts',(2.49097294870383,1.17156242527378,-2.97967994645086E-16));
#28655=CARTESIAN_POINT('Ctrl Pts',(2.522710946502,1.07849900531789,-2.19554586473301E-16));
#28656=CARTESIAN_POINT('Ctrl Pts',(2.5494811878723,0.984141912890972,-2.91433543964104E-16));
#28657=CARTESIAN_POINT('Ctrl Pts',(2.57415365468709,0.897178848216262,-3.57679909427988E-16));
#28658=CARTESIAN_POINT('Ctrl Pts',(2.59460600088325,0.809116138918699,-3.16658239360586E-16));
#28659=CARTESIAN_POINT('Ctrl Pts',(2.61059963694684,0.720255260258035,-3.60822483003176E-16));
#28660=CARTESIAN_POINT('Ctrl Pts',(2.62008388056236,0.667560662371934,-3.87011927613296E-16));
#28661=CARTESIAN_POINT('Ctrl Pts',(2.6279992974166,0.614585522567766,-5.86434132422756E-17));
#28662=CARTESIAN_POINT('Ctrl Pts',(2.63428771987185,0.561395014680878,-1.11022302462516E-16));
#28663=CARTESIAN_POINT('Ctrl Pts',(2.63631849388102,0.544217749362041,-1.27937464828616E-16));
#28664=CARTESIAN_POINT('Ctrl Pts',(2.63817971938346,0.527015146377361,-5.57610343116661E-16));
#28665=CARTESIAN_POINT('Ctrl Pts',(2.63986723376609,0.50981362072198,-5.55111512312578E-16));
#28666=CARTESIAN_POINT('Ctrl Pts',(2.64857594877992,0.421042119704249,-5.42215856095108E-16));
#28667=CARTESIAN_POINT('Ctrl Pts',(2.65267958281541,0.332167648005602,-3.9556124136452E-16));
#28668=CARTESIAN_POINT('Ctrl Pts',(2.65199707698894,0.243482089150498,-3.33066907387547E-16));
#28669=CARTESIAN_POINT('Ctrl Pts',(2.6516640117541,0.200203225671092,-3.02569453423877E-16));
#28670=CARTESIAN_POINT('Ctrl Pts',(2.65019037381467,0.156969394455165,3.29031573743661E-16));
#28671=CARTESIAN_POINT('Ctrl Pts',(2.64755062273554,0.113815198443072,3.05311331771918E-16));
#28672=CARTESIAN_POINT('Ctrl Pts',(2.64202705093324,0.0235167979128891,
2.25896251348351E-16));
#28673=CARTESIAN_POINT('Ctrl Pts',(2.63140068084878,-0.0664344653587478,
-3.57990035170166E-16));
#28674=CARTESIAN_POINT('Ctrl Pts',(2.61586718053927,-0.155705179881193,
-4.44089209850063E-16));
#28675=CARTESIAN_POINT('Ctrl Pts',(2.59996532115929,-0.247092846588728,
-5.32230127300229E-16));
#28676=CARTESIAN_POINT('Ctrl Pts',(2.57892033292169,-0.337768326694507,
-1.15896493065795E-16));
#28677=CARTESIAN_POINT('Ctrl Pts',(2.55289626581674,-0.427342175555427,
-2.77555756156289E-17));
#28678=CARTESIAN_POINT('Ctrl Pts',(2.54882874919627,-0.441342413009925,
-1.39793028591053E-17));
#28679=CARTESIAN_POINT('Ctrl Pts',(2.54463896540328,-0.455317440734485,
-3.65684696917243E-16));
#28680=CARTESIAN_POINT('Ctrl Pts',(2.54032919703339,-0.469260060669249,
-3.60822483003176E-16));
#28681=CARTESIAN_POINT('Ctrl Pts',(2.51414391528516,-0.553972602032386,
-3.31280653760249E-16));
#28682=CARTESIAN_POINT('Ctrl Pts',(2.48362384320016,-0.637202118714745,
1.1028949584026E-16));
#28683=CARTESIAN_POINT('Ctrl Pts',(2.44898771893138,-0.718649795920404,
0.));
#28684=CARTESIAN_POINT('Ctrl Pts',(2.41432501221678,-0.800159982385209,
-1.10374140546078E-16));
#28685=CARTESIAN_POINT('Ctrl Pts',(2.37553928084343,-0.879886390297083,
5.56731917103673E-17));
#28686=CARTESIAN_POINT('Ctrl Pts',(2.33280620908713,-0.957500984689981,
8.32667268468867E-17));
#28687=CARTESIAN_POINT('Ctrl Pts',(2.29068411086063,-1.0340058890758,1.10465745070182E-16));
#28688=CARTESIAN_POINT('Ctrl Pts',(2.24472605801825,-1.10845957586292,-1.45162796518328E-16));
#28689=CARTESIAN_POINT('Ctrl Pts',(2.19506803735907,-1.18050963761054,-1.66533453693773E-16));
#28690=CARTESIAN_POINT('Ctrl Pts',(2.16851747476405,-1.21903251164,-1.77959663669557E-16));
#28691=CARTESIAN_POINT('Ctrl Pts',(2.14090871133255,-1.25686754949034,-6.12242562191498E-17));
#28692=CARTESIAN_POINT('Ctrl Pts',(2.11225966440144,-1.29395535226115,-5.55111512312578E-17));
#28693=CARTESIAN_POINT('Ctrl Pts',(2.10389009111628,-1.30479023567008,-5.38421166208939E-17));
#28694=CARTESIAN_POINT('Ctrl Pts',(2.0954317221698,-1.31556131757123,-5.76575592671161E-18));
#28695=CARTESIAN_POINT('Ctrl Pts',(2.08688497852084,-1.32626704704954,0.));
#28696=CARTESIAN_POINT('Ctrl Pts',(2.07860608678634,-1.33663726276327,5.58505918105939E-18));
#28697=CARTESIAN_POINT('Ctrl Pts',(2.07025013926869,-1.34693879666623,-1.85493259861054E-16));
#28698=CARTESIAN_POINT('Ctrl Pts',(2.06181881264409,-1.35716935688295,-1.66533453693773E-16));
#28699=CARTESIAN_POINT('Ctrl Pts',(2.00758715298996,-1.42297397867583,-4.45809068463581E-17));
#28700=CARTESIAN_POINT('Ctrl Pts',(1.95022582590432,-1.48586254952678,-2.55249516657381E-17));
#28701=CARTESIAN_POINT('Ctrl Pts',(1.8898935724857,-1.54553906223415,0.));
#28702=CARTESIAN_POINT('Ctrl Pts',(1.83050776280639,-1.6042794179337,2.51245368074963E-17));
#28703=CARTESIAN_POINT('Ctrl Pts',(1.76824286709423,-1.65990821687079,-2.08086528920867E-16));
#28704=CARTESIAN_POINT('Ctrl Pts',(1.70322439968709,-1.71210071694254,-2.22044604925031E-16));
#28705=CARTESIAN_POINT('Ctrl Pts',(1.64023093603462,-1.76266767871992,-2.35567955881933E-16));
#28706=CARTESIAN_POINT('Ctrl Pts',(1.57465218130676,-1.81000934229147,8.12709303573321E-17));
#28707=CARTESIAN_POINT('Ctrl Pts',(1.50658663996491,-1.85378460546696,1.11022302462516E-16));
#28708=CARTESIAN_POINT('Ctrl Pts',(1.46434993749398,-1.88094846444582,1.2948391794277E-16));
#28709=CARTESIAN_POINT('Ctrl Pts',(1.42115540397303,-1.9067381345186,4.99167222978473E-17));
#28710=CARTESIAN_POINT('Ctrl Pts',(1.37702479013104,-1.93106208855763,5.55111512312578E-17));
#28711=CARTESIAN_POINT('Ctrl Pts',(0.260898964428461,2.9250678849183,19.058));
#28712=CARTESIAN_POINT('Ctrl Pts',(0.726863739861969,2.88429659618081,19.0328104438584));
#28713=CARTESIAN_POINT('Ctrl Pts',(1.18340500184494,2.7384933202854,19.0076208877168));
#28714=CARTESIAN_POINT('Ctrl Pts',(1.57541514848214,2.49092003235782,18.9824313315753));
#28715=CARTESIAN_POINT('Ctrl Pts',(2.39655179416664,1.97233269232634,18.929667218672));
#28716=CARTESIAN_POINT('Ctrl Pts',(2.93454570444379,1.00720976345797,18.8769031057688));
#28717=CARTESIAN_POINT('Ctrl Pts',(2.94628683933111,0.0361474094946818,
18.8241389928656));
#28718=CARTESIAN_POINT('Ctrl Pts',(2.95802797421842,-0.934914944468595,
18.7713748799624));
#28719=CARTESIAN_POINT('Ctrl Pts',(2.44351633371593,-1.9119167235268,18.7186107670591));
#28720=CARTESIAN_POINT('Ctrl Pts',(1.63604360338806,-2.45085804146298,18.6658466541559));
#28721=CARTESIAN_POINT('Ctrl Pts',(0.828570873060194,-2.98979935939915,
18.6130825412527));
#28722=CARTESIAN_POINT('Ctrl Pts',(-0.271862947093059,-3.09068021621329,
18.5603184283495));
#28723=CARTESIAN_POINT('Ctrl Pts',(-1.16394092644999,-2.70723224004173,
18.5075543154462));
#28724=CARTESIAN_POINT('Ctrl Pts',(-2.05601890580693,-2.32378426387017,
18.454790202543));
#28725=CARTESIAN_POINT('Ctrl Pts',(-2.73974104436754,-1.45600745471292,
18.4020260896398));
#28726=CARTESIAN_POINT('Ctrl Pts',(-2.9041551334136,-0.499050683143429,
18.3492619767365));
#28727=CARTESIAN_POINT('Ctrl Pts',(-2.93228850345654,-0.335303043717479,
18.3402333568542));
#28728=CARTESIAN_POINT('Ctrl Pts',(-2.94521673044455,-0.168944248759899,
18.3312047369719));
#28729=CARTESIAN_POINT('Ctrl Pts',(-2.94374845943093,-0.00235935217182681,
18.3221761170896));
#28730=CARTESIAN_POINT('Origin',(0.,0.,-1.84858989190501));
#28731=CARTESIAN_POINT('',(-1.37702479013099,-1.93106208855767,0.));
#28732=CARTESIAN_POINT('Ctrl Pts',(-1.37997554054992,-1.93359434039962,
-2.49583340106163E-15));
#28733=CARTESIAN_POINT('Ctrl Pts',(-0.789677438324666,-2.34979595234001,
0.0486480664188813));
#28734=CARTESIAN_POINT('Ctrl Pts',(0.870549345642383,-2.62706253801033,
0.150093709533546));
#28735=CARTESIAN_POINT('Ctrl Pts',(2.69329736340148,-0.769327930944301,
0.304336929343994));
#28736=CARTESIAN_POINT('Ctrl Pts',(2.11117816219839,1.84124601305982,0.462729659431337));
#28737=CARTESIAN_POINT('Ctrl Pts',(-0.39528737250602,2.77289693006155,0.621122389518683));
#28738=CARTESIAN_POINT('Ctrl Pts',(-2.13794957738225,1.47774671669238,0.749742467009907));
#28739=CARTESIAN_POINT('Ctrl Pts',(-2.36920067152979,0.345159485015423,
0.825564967805353));
#28740=CARTESIAN_POINT('Ctrl Pts',(-2.36815429608612,0.000817443606317657,
0.848589891905016));
#28741=CARTESIAN_POINT('Origin',(0.,0.,0.));
#28742=CARTESIAN_POINT('Ctrl Pts',(-1.03908919352509,2.13201587949044,-0.329233991005384));
#28743=CARTESIAN_POINT('Ctrl Pts',(-1.74635765611394,1.78731159118428,-0.276436414309603));
#28744=CARTESIAN_POINT('Ctrl Pts',(-2.77891474382729,0.344899083844066,
-0.17084126091804));
#28745=CARTESIAN_POINT('Ctrl Pts',(-1.80015933390001,-2.14838790817324,
-0.0124485308306951));
#28746=CARTESIAN_POINT('Ctrl Pts',(0.821513079145993,-2.67704002715534,
0.145944199256649));
#28747=CARTESIAN_POINT('Ctrl Pts',(2.69329736340148,-0.769327930944301,
0.304336929343994));
#28748=CARTESIAN_POINT('Ctrl Pts',(2.11117816219839,1.84124601305982,0.462729659431337));
#28749=CARTESIAN_POINT('Ctrl Pts',(-0.39528737250602,2.77289693006155,0.621122389518683));
#28750=CARTESIAN_POINT('Ctrl Pts',(-2.54133664906011,1.1779485971876,0.779515119606025));
#28751=CARTESIAN_POINT('Ctrl Pts',(-2.37143388856986,-1.49076941799294,
0.937907849693373));
#28752=CARTESIAN_POINT('Ctrl Pts',(-0.0402824848387021,-2.80074754850057,
1.09630057978071));
#28753=CARTESIAN_POINT('Ctrl Pts',(2.32755559974952,-1.55833818967747,1.25469330986806));
#28754=CARTESIAN_POINT('Ctrl Pts',(2.57419348860935,1.10429523958194,1.4130860399554));
#28755=CARTESIAN_POINT('Ctrl Pts',(0.474838546093255,2.76051273114501,1.57147877004275));
#28756=CARTESIAN_POINT('Ctrl Pts',(-2.05725600774418,1.90095227802787,1.72987150013009));
#28757=CARTESIAN_POINT('Ctrl Pts',(-2.71447628777791,-0.691042339108541,
1.88826423021744));
#28758=CARTESIAN_POINT('Ctrl Pts',(-0.897863084978552,-2.65325422541087,
2.04665696030478));
#28759=CARTESIAN_POINT('Ctrl Pts',(1.7370153276097,-2.19742960924133,2.20504969039212));
#28760=CARTESIAN_POINT('Ctrl Pts',(2.78886857766781,0.261018802222555,2.36344242047947));
#28761=CARTESIAN_POINT('Ctrl Pts',(1.29909191311228,2.48158786740548,2.52183515056681));
#28762=CARTESIAN_POINT('Ctrl Pts',(-1.37460948338166,2.44056701717432,2.68022788065416));
#28763=CARTESIAN_POINT('Ctrl Pts',(-2.79556332719592,0.175340213572512,
2.8386206107415));
#28764=CARTESIAN_POINT('Ctrl Pts',(-1.6687861293442,-2.24968248607005,2.99701334082885));
#28765=CARTESIAN_POINT('Ctrl Pts',(0.978835944215164,-2.62446160086853,
3.15540607091619));
#28766=CARTESIAN_POINT('Ctrl Pts',(2.73439785209926,-0.607442893388946,
3.31379880100354));
#28767=CARTESIAN_POINT('Ctrl Pts',(1.99797176831316,1.9631676666159,3.47219153109088));
#28768=CARTESIAN_POINT('Ctrl Pts',(-0.559301870866465,2.7446493220368,3.63058426117822));
#28769=CARTESIAN_POINT('Ctrl Pts',(-2.60685687452164,1.02480032995442,3.78897699126557));
#28770=CARTESIAN_POINT('Ctrl Pts',(-2.27865810264075,-1.62899838275098,
3.94736972135291));
#28771=CARTESIAN_POINT('Ctrl Pts',(0.126191152782097,-2.79821269277661,
4.10576245144026));
#28772=CARTESIAN_POINT('Ctrl Pts',(2.41603635476259,-1.41728148685534,4.26415518152759));
#28773=CARTESIAN_POINT('Ctrl Pts',(2.50403167886292,1.25528635446798,4.42254791161495));
#28774=CARTESIAN_POINT('Ctrl Pts',(0.309982763347203,2.78385149874581,4.58094064170228));
#28775=CARTESIAN_POINT('Ctrl Pts',(-2.16656832077059,1.77535917267124,4.73933337178964));
#28776=CARTESIAN_POINT('Ctrl Pts',(-2.66862171862793,-0.851103168495116,
4.89772610187697));
#28777=CARTESIAN_POINT('Ctrl Pts',(-0.738632074782922,-2.7019143470289,
5.05611883196433));
#28778=CARTESIAN_POINT('Ctrl Pts',(1.86450842642192,-2.09034131384488,5.21451156205166));
#28779=CARTESIAN_POINT('Ctrl Pts',(2.76843291921558,0.426260075974678,5.37290429213902));
#28780=CARTESIAN_POINT('Ctrl Pts',(1.14935163317956,2.55439020196149,5.53129702222635));
#28781=CARTESIAN_POINT('Ctrl Pts',(-1.51718895457673,2.35458194945041,5.68968975231371));
#28782=CARTESIAN_POINT('Ctrl Pts',(-2.80104243678463,0.00893016793130419,
5.84808248240103));
#28783=CARTESIAN_POINT('Ctrl Pts',(-1.53217152184201,-2.34486010419053,
6.0064752124884));
#28784=CARTESIAN_POINT('Ctrl Pts',(1.13304083122442,-2.56166683144901,6.16486794257572));
#28785=CARTESIAN_POINT('Ctrl Pts',(2.76565869916243,-0.443903638546721,
6.32326067266308));
#28786=CARTESIAN_POINT('Ctrl Pts',(1.87779906814186,2.07841024349223,6.48165340275042));
#28787=CARTESIAN_POINT('Ctrl Pts',(-0.721388970917745,2.70656912588725,
6.64004613283776));
#28788=CARTESIAN_POINT('Ctrl Pts',(-2.66314062068401,0.868101673210355,
6.79843886292512));
#28789=CARTESIAN_POINT('Ctrl Pts',(-2.17784441634251,-1.76150849523174,
6.95683159301245));
#28790=CARTESIAN_POINT('Ctrl Pts',(0.292225921295444,-2.78577143561543,
7.11522432309981));
#28791=CARTESIAN_POINT('Ctrl Pts',(2.49597675267592,-1.27122717508287,7.27361705318714));
#28792=CARTESIAN_POINT('Ctrl Pts',(2.42502418520658,1.40184741742138,7.43200978327449));
#28793=CARTESIAN_POINT('Ctrl Pts',(0.144030698698804,2.79735118252968,7.59040251336184));
#28794=CARTESIAN_POINT('Ctrl Pts',(-2.26822487569406,1.64349456763645,7.74879524344916));
#28795=CARTESIAN_POINT('Ctrl Pts',(-2.61333826674507,-1.00815751950462,
7.90718797353653));
#28796=CARTESIAN_POINT('Ctrl Pts',(-0.576791078891976,-2.74102727674834,
8.06558070362385));
#28797=CARTESIAN_POINT('Ctrl Pts',(1.9854134998704,-1.97586733236324,8.22397343371122));
#28798=CARTESIAN_POINT('Ctrl Pts',(2.73821547444757,0.589995335628766,8.38236616379854));
#28799=CARTESIAN_POINT('Ctrl Pts',(0.995550277773485,2.61816693986326,8.54075889388591));
#28800=CARTESIAN_POINT('Ctrl Pts',(-1.65440766437566,2.26027736364875,8.69915162397323));
#28801=CARTESIAN_POINT('Ctrl Pts',(-2.79662450548933,-0.15751144677259,
8.85754435406059));
#28802=CARTESIAN_POINT('Ctrl Pts',(-1.39014322226223,-2.43175251663614,
9.01593708414793));
#28803=CARTESIAN_POINT('Ctrl Pts',(1.2832422936176,-2.48982081613093,9.17432981423527));
#28804=CARTESIAN_POINT('Ctrl Pts',(2.78714752338885,-0.278795917178183,
9.33272254432263));
#28805=CARTESIAN_POINT('Ctrl Pts',(1.75099145741626,2.18630908076216,9.49111527440996));
#28806=CARTESIAN_POINT('Ctrl Pts',(-0.880927155331511,2.6589256904937,9.64950800449731));
#28807=CARTESIAN_POINT('Ctrl Pts',(-2.71001457495083,0.708335714278131,
9.80790073458465));
#28808=CARTESIAN_POINT('Ctrl Pts',(-2.06933565641643,-1.88779459201775,
9.966293464672));
#28809=CARTESIAN_POINT('Ctrl Pts',(0.457228155062243,-2.76348708967243,
10.1246861947593));
#28810=CARTESIAN_POINT('Ctrl Pts',(2.56709800604834,-1.12068118031423,10.2830789248467));
#28811=CARTESIAN_POINT('Ctrl Pts',(2.33744824681434,1.54345527114731,10.441471654934));
#28812=CARTESIAN_POINT('Ctrl Pts',(-0.0224302759543461,2.80096686222604,
10.5998643850214));
#28813=CARTESIAN_POINT('Ctrl Pts',(-2.36186701179702,1.5058229308763,10.7582571151087));
#28814=CARTESIAN_POINT('Ctrl Pts',(-2.54882099169811,-1.16164970315792,
10.9166498451961));
#28815=CARTESIAN_POINT('Ctrl Pts',(-0.412912081686591,-2.77045521410563,
11.0750425752834));
#28816=CARTESIAN_POINT('Ctrl Pts',(2.09930342438264,-1.85441193183801,11.2334353053708));
#28817=CARTESIAN_POINT('Ctrl Pts',(2.69832297238025,0.751645938785551,11.3918280354581));
#28818=CARTESIAN_POINT('Ctrl Pts',(0.838231300737091,2.67269279323914,11.5502207655454));
#28819=CARTESIAN_POINT('Ctrl Pts',(-1.78578078273074,2.15798644031825,11.7086134956328));
#28820=CARTESIAN_POINT('Ctrl Pts',(-2.78232513769374,-0.323396519346309,
11.8670062257201));
#28821=CARTESIAN_POINT('Ctrl Pts',(-1.24320306842743,-2.51005271084502,
12.0253989558075));
#28822=CARTESIAN_POINT('Ctrl Pts',(1.42890961951376,-2.40917740729671,12.1837916858948));
#28823=CARTESIAN_POINT('Ctrl Pts',(2.79878839655315,-0.112703113920128,
12.3421844159822));
#28824=CARTESIAN_POINT('Ctrl Pts',(1.61799699147824,2.28648293589416,12.5005771460695));
#28825=CARTESIAN_POINT('Ctrl Pts',(-1.03735272104025,2.60188735588576,12.6589698761568));
#28826=CARTESIAN_POINT('Ctrl Pts',(-2.7473131153984,0.546066961578709,12.8173626062442));
#28827=CARTESIAN_POINT('Ctrl Pts',(-1.95351522170293,-2.00741046105244,
12.9757553363315));
#28828=CARTESIAN_POINT('Ctrl Pts',(0.620614844457064,-2.73143839311951,
13.1341480664189));
#28829=CARTESIAN_POINT('Ctrl Pts',(2.62914881900703,-0.966175433387754,
13.2925407965062));
#28830=CARTESIAN_POINT('Ctrl Pts',(2.24161329961403,1.67960956640559,13.4509335265936));
#28831=CARTESIAN_POINT('Ctrl Pts',(-0.18881199672574,2.79468576238185,13.6093262566809));
#28832=CARTESIAN_POINT('Ctrl Pts',(-2.44716385919473,1.36283070365345,13.7677189867683));
#28833=CARTESIAN_POINT('Ctrl Pts',(-2.47529785521649,-1.31103737876807,
13.9261117168556));
#28834=CARTESIAN_POINT('Ctrl Pts',(-0.247574124043378,-2.79009418007158,
14.084504446943));
#28835=CARTESIAN_POINT('Ctrl Pts',(2.20577578767506,-1.72640425598558,14.2428971770303));
#28836=CARTESIAN_POINT('Ctrl Pts',(2.64889636694473,0.910640718254001,14.4012899071176));
#28837=CARTESIAN_POINT('Ctrl Pts',(0.677950564144521,2.71777510348644,14.559682637205));
#28838=CARTESIAN_POINT('Ctrl Pts',(-1.91084412322983,2.04807060848979,14.7180753672923));
#28839=CARTESIAN_POINT('Ctrl Pts',(-2.75819485796213,-0.488138920773397,
14.8764680973797));
#28840=CARTESIAN_POINT('Ctrl Pts',(-1.09187025049414,-2.57948402526614,
15.034860827467));
#28841=CARTESIAN_POINT('Ctrl Pts',(1.56952811621541,-2.32002154590554,15.1932535575544));
#28842=CARTESIAN_POINT('Ctrl Pts',(2.80054018729513,0.0537879083119886,
15.3516462876417));
#28843=CARTESIAN_POINT('Ctrl Pts',(1.47928558581743,2.37857786000547,15.510039017729));
#28844=CARTESIAN_POINT('Ctrl Pts',(-1.19011296325406,2.53565565848489,15.6684317478164));
#28845=CARTESIAN_POINT('Ctrl Pts',(-2.77490445240338,0.381868765748693,
15.8268244779037));
#28846=CARTESIAN_POINT('Ctrl Pts',(-1.83079234764519,-2.11993345699756,
15.9852172079911));
#28847=CARTESIAN_POINT('Ctrl Pts',(0.781808691918871,-2.68973858755105,
16.1436099380784));
#28848=CARTESIAN_POINT('Ctrl Pts',(2.68190993738254,-0.808255851442284,
16.3020026681657));
#28849=CARTESIAN_POINT('Ctrl Pts',(2.137857975385,1.80982921402577,16.4603953982531));
#28850=CARTESIAN_POINT('Ctrl Pts',(-0.354526606378597,2.77853009386107,
16.6187881283404));
#28851=CARTESIAN_POINT('Ctrl Pts',(-2.52381398393833,1.21502309313244,16.7771808584278));
#28852=CARTESIAN_POINT('Ctrl Pts',(-2.39302873693005,-1.45579264417825,
16.9355735885151));
#28853=CARTESIAN_POINT('Ctrl Pts',(-0.0813612164248821,-2.79987490584551,
17.0939663186025));
#28854=CARTESIAN_POINT('Ctrl Pts',(2.3044540321531,-1.59229636617095,17.2523590486898));
#28855=CARTESIAN_POINT('Ctrl Pts',(2.59011097558326,1.0664174443023,17.4107517787772));
#28856=CARTESIAN_POINT('Ctrl Pts',(0.515273103550636,2.75325543193802,17.5691445088645));
#28857=CARTESIAN_POINT('Ctrl Pts',(-2.02915332780205,1.93091661030183,17.7275372389519));
#28858=CARTESIAN_POINT('Ctrl Pts',(-2.72432363673881,-0.651153449862876,
17.8859299690392));
#28859=CARTESIAN_POINT('Ctrl Pts',(-0.936670484863442,-2.63980707365487,
18.0443226991266));
#28860=CARTESIAN_POINT('Ctrl Pts',(1.70458375322942,-2.22265690947637,18.2027154292139));
#28861=CARTESIAN_POINT('Ctrl Pts',(2.7924295091237,0.220067221674903,18.3611081593012));
#28862=CARTESIAN_POINT('Ctrl Pts',(1.33528471034559,2.46230981068379,18.5195008893886));
#28863=CARTESIAN_POINT('Ctrl Pts',(-1.33854848928615,2.46038562697746,18.6778936194759));
#28864=CARTESIAN_POINT('Ctrl Pts',(-2.79291960316285,0.216472177012814,
18.8362863495633));
#28865=CARTESIAN_POINT('Ctrl Pts',(-1.7011639917225,-2.22525441833135,18.9946790796506));
#28866=CARTESIAN_POINT('Ctrl Pts',(0.939403752255799,-2.63798173542721,
19.153071809738));
#28867=CARTESIAN_POINT('Ctrl Pts',(2.72681418428107,-0.648558891555657,
19.3114645398253));
#28868=CARTESIAN_POINT('Ctrl Pts',(2.02326260265721,1.93590572399224,19.4698572699127));
#28869=CARTESIAN_POINT('Ctrl Pts',(0.333728659905137,2.4764638032096,19.5754524233042));
#28870=CARTESIAN_POINT('Ctrl Pts',(-0.439445221994122,2.33068358199189,
19.62825));
#28871=CARTESIAN_POINT('Ctrl Pts',(-1.12236674703447,2.30288577939268,-0.219489327336923));
#28872=CARTESIAN_POINT('Ctrl Pts',(-1.88631907045622,1.93055524880318,-0.166691750641141));
#28873=CARTESIAN_POINT('Ctrl Pts',(-3.00163019762969,0.372540937968967,
-0.0610965972495787));
#28874=CARTESIAN_POINT('Ctrl Pts',(-1.94443267076893,-2.32056994037671,
0.0972961328377661));
#28875=CARTESIAN_POINT('Ctrl Pts',(0.887353047296498,-2.8915907562914,0.25568886292511));
#28876=CARTESIAN_POINT('Ctrl Pts',(2.90915103284102,-0.830985532942982,
0.414081593012455));
#28877=CARTESIAN_POINT('Ctrl Pts',(2.28037802825984,1.98881223194844,0.572474323099799));
#28878=CARTESIAN_POINT('Ctrl Pts',(-0.426967583907085,2.995130087627,0.730867053187144));
#28879=CARTESIAN_POINT('Ctrl Pts',(-2.745011463596,1.27235500420722,0.889259783274488));
#28880=CARTESIAN_POINT('Ctrl Pts',(-2.56149188722866,-1.61024677446114,
1.04765251336183));
#28881=CARTESIAN_POINT('Ctrl Pts',(-0.0435109148979961,-3.02521278718262,
1.20604524344918));
#28882=CARTESIAN_POINT('Ctrl Pts',(2.51409698350372,-1.68323082910176,1.36443797353652));
#28883=CARTESIAN_POINT('Ctrl Pts',(2.78050160664871,1.19279871597019,1.52283070362387));
#28884=CARTESIAN_POINT('Ctrl Pts',(0.512894367169087,2.98175336006676,1.68122343371121));
#28885=CARTESIAN_POINT('Ctrl Pts',(-2.2221342957054,2.05330364116276,1.83961616379856));
#28886=CARTESIAN_POINT('Ctrl Pts',(-2.93202733701797,-0.74642576117755,
1.9980088938859));
#28887=CARTESIAN_POINT('Ctrl Pts',(-0.969822105984018,-2.86589864718671,
2.15640162397324));
#28888=CARTESIAN_POINT('Ctrl Pts',(1.87622800328088,-2.37354207678217,2.31479435406059));
#28889=CARTESIAN_POINT('Ctrl Pts',(3.01238177908942,0.281938091350456,2.47318708414793));
#28890=CARTESIAN_POINT('Ctrl Pts',(1.40320732205116,2.68047413020551,2.63157981423527));
#28891=CARTESIAN_POINT('Ctrl Pts',(-1.48477722982743,2.63616567379829,2.78997254432262));
#28892=CARTESIAN_POINT('Ctrl Pts',(-3.01961307770834,0.189392812819178,
2.94836527440996));
#28893=CARTESIAN_POINT('Ctrl Pts',(-1.80253059232985,-2.42998274785725,
3.10675800449731));
#28894=CARTESIAN_POINT('Ctrl Pts',(1.05728451554978,-2.83479844467519,3.26515073458465));
#28895=CARTESIAN_POINT('Ctrl Pts',(2.95354551032062,-0.656126257986841,
3.423543464672));
#28896=CARTESIAN_POINT('Ctrl Pts',(2.15809873516333,2.12050526710607,3.58193619475934));
#28897=CARTESIAN_POINT('Ctrl Pts',(-0.604126984792399,2.96461858185079,
3.74032892484669));
#28898=CARTESIAN_POINT('Ctrl Pts',(-2.81578279176923,1.1069327059295,3.89872165493403));
#28899=CARTESIAN_POINT('Ctrl Pts',(-2.46128060824926,-1.75955406635503,
4.05711438502138));
#28900=CARTESIAN_POINT('Ctrl Pts',(0.136304712372256,-3.0224747760563,4.21550711510872));
#28901=CARTESIAN_POINT('Ctrl Pts',(2.60966900734729,-1.53086917075673,4.37389984519606));
#28902=CARTESIAN_POINT('Ctrl Pts',(2.70471669553439,1.35589097744473,4.5322925752834));
#28903=CARTESIAN_POINT('Ctrl Pts',(0.334826257363418,3.00696260758384,4.69068530537076));
#28904=CARTESIAN_POINT('Ctrl Pts',(-2.3402074177692,1.91764490658303,4.8490780354581));
#28905=CARTESIAN_POINT('Ctrl Pts',(-2.88249776445171,-0.919314627239958,
5.00747076554544));
#28906=CARTESIAN_POINT('Ctrl Pts',(-0.797829564772043,-2.91845862254883,
5.16586349563279));
#28907=CARTESIAN_POINT('Ctrl Pts',(2.01393900583474,-2.25787121570639,5.32425622572012));
#28908=CARTESIAN_POINT('Ctrl Pts',(2.9903083097054,0.460422587246163,5.48264895580748));
#28909=CARTESIAN_POINT('Ctrl Pts',(1.24146614339645,2.75911119035523,5.64104168589481));
#28910=CARTESIAN_POINT('Ctrl Pts',(-1.63878369845042,2.54328935350145,5.79943441598217));
#28911=CARTESIAN_POINT('Ctrl Pts',(-3.02553130921729,0.00964587409243157,
5.9578271460695));
#28912=CARTESIAN_POINT('Ctrl Pts',(-1.65496703996583,-2.53278835329135,
6.11621987615686));
#28913=CARTESIAN_POINT('Ctrl Pts',(1.22384811614141,-2.76697100356297,6.27461260624418));
#28914=CARTESIAN_POINT('Ctrl Pts',(2.9873117504533,-0.47948018889722,6.43300533633155));
#28915=CARTESIAN_POINT('Ctrl Pts',(2.02829482283888,2.24498393258978,6.59139806641888));
#28916=CARTESIAN_POINT('Ctrl Pts',(-0.7792045164946,2.92348645753929,6.74979079650623));
#28917=CARTESIAN_POINT('Ctrl Pts',(-2.87657738523129,0.937675473027413,
6.90818352659357));
#28918=CARTESIAN_POINT('Ctrl Pts',(-2.3523872333088,-1.90268416993127,7.06657625668092));
#28919=CARTESIAN_POINT('Ctrl Pts',(0.315646297475985,-3.00903641733213,
7.22496898676826));
#28920=CARTESIAN_POINT('Ctrl Pts',(2.69601620922536,-1.37310937129398,7.38336171685561));
#28921=CARTESIAN_POINT('Ctrl Pts',(2.61937716530061,1.51419814153992,7.54175444694295));
#28922=CARTESIAN_POINT('Ctrl Pts',(0.155574004406001,3.02154422027783,7.7001471770303));
#28923=CARTESIAN_POINT('Ctrl Pts',(-2.45001121283815,1.77521204449176,7.85853990711763));
#28924=CARTESIAN_POINT('Ctrl Pts',(-2.82278363361361,-1.08895606143883,
8.01693263720499));
#28925=CARTESIAN_POINT('Ctrl Pts',(-0.623017861188913,-2.9607062486138,
8.17532536729232));
#28926=CARTESIAN_POINT('Ctrl Pts',(2.14453398731652,-2.13422274451042,8.33371809737967));
#28927=CARTESIAN_POINT('Ctrl Pts',(2.95766909509389,0.637280369906155,8.49211082746702));
#28928=CARTESIAN_POINT('Ctrl Pts',(1.07533841535129,2.82799929957753,8.65050355755435));
#28929=CARTESIAN_POINT('Ctrl Pts',(-1.78699976874446,2.4414267493514,8.8088962876417));
#28930=CARTESIAN_POINT('Ctrl Pts',(-3.02075930388085,-0.170135163791943,
8.96728901772905));
#28931=CARTESIAN_POINT('Ctrl Pts',(-1.50155591647468,-2.62664473723439,
9.12568174781639));
#28932=CARTESIAN_POINT('Ctrl Pts',(1.38608743861396,-2.68936690662652,9.28407447790374));
#28933=CARTESIAN_POINT('Ctrl Pts',(3.01052279132919,-0.301139948908758,
9.44246720799109));
#28934=CARTESIAN_POINT('Ctrl Pts',(1.89132424664949,2.36153029622255,9.60085993807842));
#28935=CARTESIAN_POINT('Ctrl Pts',(-0.95152885032855,2.87202465047459,9.75925266816578));
#28936=CARTESIAN_POINT('Ctrl Pts',(-2.92720804128942,0.765105109741005,
9.9176453982531));
#28937=CARTESIAN_POINT('Ctrl Pts',(-2.23518206491529,-2.03909143557181,
10.0760381283405));
#28938=CARTESIAN_POINT('Ctrl Pts',(0.493872595584237,-2.98496609784301,
10.2344308584278));
#28939=CARTESIAN_POINT('Ctrl Pts',(2.77283745834433,-1.2104979039816,10.3928235885152));
#28940=CARTESIAN_POINT('Ctrl Pts',(2.52478247438834,1.66715512264539,10.5512163186025));
#28941=CARTESIAN_POINT('Ctrl Pts',(-0.0242279450261061,3.02544967775387,
10.7096090486898));
#28942=CARTESIAN_POINT('Ctrl Pts',(-2.55115827541772,1.62650674751413,10.8680017787772));
#28943=CARTESIAN_POINT('Ctrl Pts',(-2.75309563707472,-1.25474983923546,
11.0263945088645));
#28944=CARTESIAN_POINT('Ctrl Pts',(-0.446004821166146,-2.99249268093304,
11.1847872389519));
#28945=CARTESIAN_POINT('Ctrl Pts',(2.26755159243775,-2.00303333012067,11.3431799690392));
#28946=CARTESIAN_POINT('Ctrl Pts',(2.91457941804272,0.811886421775233,11.5015726991266));
#28947=CARTESIAN_POINT('Ctrl Pts',(0.905411146736239,2.88689511435851,11.6599654292139));
#28948=CARTESIAN_POINT('Ctrl Pts',(-1.92890175407427,2.33093774457201,11.8183581593013));
#28949=CARTESIAN_POINT('Ctrl Pts',(-3.00531391669236,-0.349315055610967,
11.9767508893886));
#28950=CARTESIAN_POINT('Ctrl Pts',(-1.34283927935057,-2.71122028167659,
12.1351436194759));
#28951=CARTESIAN_POINT('Ctrl Pts',(1.54342923731041,-2.60226035118638,12.2935363495633));
#28952=CARTESIAN_POINT('Ctrl Pts',(3.02309661947356,-0.121735677879665,
12.4519290796506));
#28953=CARTESIAN_POINT('Ctrl Pts',(1.74767097122464,2.46973256088184,12.610321809738));
#28954=CARTESIAN_POINT('Ctrl Pts',(-1.12049110537995,2.81041499225748,12.7687145398253));
#28955=CARTESIAN_POINT('Ctrl Pts',(-2.9674958642907,0.589831366882863,12.9271072699127));
#28956=CARTESIAN_POINT('Ctrl Pts',(-2.11007922931703,-2.16829388966213,
13.0855));
#28957=CARTESIAN_POINT('Ctrl Pts',(0.670353871905365,-2.95034886621271,
13.2438927300873));
#28958=CARTESIAN_POINT('Ctrl Pts',(2.83986131878408,-1.04360933112704,13.4022854601747));
#28959=CARTESIAN_POINT('Ctrl Pts',(2.4212668583934,1.81422147115141,13.560678190262));
#28960=CARTESIAN_POINT('Ctrl Pts',(-0.203944288793164,3.01866518067329,
13.7190709203494));
#28961=CARTESIAN_POINT('Ctrl Pts',(-2.64329121813584,1.47205444263079,13.8774636504367));
#28962=CARTESIAN_POINT('Ctrl Pts',(-2.67368000650243,-1.41611015417897,
14.0358563805241));
#28963=CARTESIAN_POINT('Ctrl Pts',(-0.267415892672147,-3.01370560710306,
14.1942491106114));
#28964=CARTESIAN_POINT('Ctrl Pts',(2.38255715767915,-1.86476650987348,14.3526418406987));
#28965=CARTESIAN_POINT('Ctrl Pts',(2.86119152920189,0.983623799605217,14.5110345707861));
#28966=CARTESIAN_POINT('Ctrl Pts',(0.732284749057705,2.93559053551808,14.6694273008734));
#28967=CARTESIAN_POINT('Ctrl Pts',(-2.06398826591936,2.21221273483691,14.8278200309608));
#28968=CARTESIAN_POINT('Ctrl Pts',(-2.9792497214951,-0.527260697179135,
14.9862127610481));
#28969=CARTESIAN_POINT('Ctrl Pts',(-1.17937792912025,-2.78621615209345,
15.1446054911355));
#28970=CARTESIAN_POINT('Ctrl Pts',(1.69531756961083,-2.50595911472641,15.3029982212228));
#28971=CARTESIAN_POINT('Ctrl Pts',(3.02498880706324,0.0580987272874007,
15.4613909513102));
#28972=CARTESIAN_POINT('Ctrl Pts',(1.59784257331787,2.5692084105368,15.6197836813975));
#28973=CARTESIAN_POINT('Ctrl Pts',(-1.28549428046646,2.73887517139744,15.7781764114849));
#28974=CARTESIAN_POINT('Ctrl Pts',(-2.9972985023641,0.412473546138461,15.9365691415722));
#28975=CARTESIAN_POINT('Ctrl Pts',(-1.97752076003333,-2.28983501405497,
16.0949618716595));
#28976=CARTESIAN_POINT('Ctrl Pts',(0.844466561504143,-2.90530703975596,
16.2533546017469));
#28977=CARTESIAN_POINT('Ctrl Pts',(2.89685096430251,-0.873033322266933,
16.4117473318342));
#28978=CARTESIAN_POINT('Ctrl Pts',(2.30919608865767,1.95487754111169,16.5701400619216));
#28979=CARTESIAN_POINT('Ctrl Pts',(-0.382940055981533,3.00121471998444,
16.7285327920089));
#28980=CARTESIAN_POINT('Ctrl Pts',(-2.72608444869231,1.31240082671298,16.8869255220963));
#28981=CARTESIAN_POINT('Ctrl Pts',(-2.58481744951702,-1.57246679552115,
17.0453182521836));
#28982=CARTESIAN_POINT('Ctrl Pts',(-0.0878818915475249,-3.02427020679184,
17.203710982271));
#28983=CARTESIAN_POINT('Ctrl Pts',(2.48914394632831,-1.71991057548322,17.3621037123583));
#28984=CARTESIAN_POINT('Ctrl Pts',(2.79769479678791,1.15188521389764,17.5204964424456));
#28985=CARTESIAN_POINT('Ctrl Pts',(0.55656954250919,2.97391442636023,17.678889172533));
#28986=CARTESIAN_POINT('Ctrl Pts',(-2.19177933323813,2.08566945764025,17.8372819026204));
#28987=CARTESIAN_POINT('Ctrl Pts',(-2.94266389939302,-0.703339986496753,
17.9956746327076));
#28988=CARTESIAN_POINT('Ctrl Pts',(-1.01173971559932,-2.85137377668732,
18.1540673627951));
#28989=CARTESIAN_POINT('Ctrl Pts',(1.84119720817182,-2.40079121292726,18.3124600928823));
#28990=CARTESIAN_POINT('Ctrl Pts',(3.01622810054042,0.237704456228855,18.4708528229697));
#28991=CARTESIAN_POINT('Ctrl Pts',(1.4423007823142,2.65965103826431,18.629245553057));
#28992=CARTESIAN_POINT('Ctrl Pts',(-1.44582613603297,2.65757264131764,18.7876382831444));
#28993=CARTESIAN_POINT('Ctrl Pts',(-3.01675747304847,0.233821287576979,
18.9460310132317));
#28994=CARTESIAN_POINT('Ctrl Pts',(-1.83750337070143,-2.40359689850469,
19.1044237433191));
#28995=CARTESIAN_POINT('Ctrl Pts',(1.01469204004945,-2.84940214716642,19.2628164734064));
#28996=CARTESIAN_POINT('Ctrl Pts',(2.94535405126905,-0.700537487938037,
19.4212092034938));
#28997=CARTESIAN_POINT('Ctrl Pts',(2.18541649734332,2.09105842264745,19.5796019335811));
#28998=CARTESIAN_POINT('Ctrl Pts',(0.360475263089987,2.67493939911702,19.6851970869727));
#28999=CARTESIAN_POINT('Ctrl Pts',(-0.474664453622252,2.51747565713062,
19.7379946636685));
#29000=CARTESIAN_POINT('Ctrl Pts',(-1.20564430054384,2.47375567929493,-0.109744663668461));
#29001=CARTESIAN_POINT('Ctrl Pts',(-2.02628048479849,2.07379890642209,-0.0569470869726798));
#29002=CARTESIAN_POINT('Ctrl Pts',(-3.22434565143208,0.400182792093866,
0.0486480664188827));
#29003=CARTESIAN_POINT('Ctrl Pts',(-2.08870600763785,-2.49275197258017,
0.207040796506227));
#29004=CARTESIAN_POINT('Ctrl Pts',(0.953193015447007,-3.10614148542747,
0.365433526593571));
#29005=CARTESIAN_POINT('Ctrl Pts',(3.12500470228055,-0.892643134941659,
0.523826256680916));
#29006=CARTESIAN_POINT('Ctrl Pts',(2.44957789432129,2.13637845083706,0.68221898676826));
#29007=CARTESIAN_POINT('Ctrl Pts',(-0.458647795308153,3.21736324519246,
0.840611716855605));
#29008=CARTESIAN_POINT('Ctrl Pts',(-2.94868627813188,1.36676141122684,0.999004446942949));
#29009=CARTESIAN_POINT('Ctrl Pts',(-2.75154988588746,-1.72972413092935,
1.15739717703029));
#29010=CARTESIAN_POINT('Ctrl Pts',(-0.0467393449572904,-3.24967802586467,
1.31578990711764));
#29011=CARTESIAN_POINT('Ctrl Pts',(2.70063836725792,-1.80812346852605,1.47418263720498));
#29012=CARTESIAN_POINT('Ctrl Pts',(2.98680972468806,1.28130219235844,1.63257536729233));
#29013=CARTESIAN_POINT('Ctrl Pts',(0.550950188244917,3.2029939889885,1.79096809737967));
#29014=CARTESIAN_POINT('Ctrl Pts',(-2.38701258366662,2.20565500429764,1.94936082746702));
#29015=CARTESIAN_POINT('Ctrl Pts',(-3.14957838625804,-0.80180918324656,
2.10775355755436));
#29016=CARTESIAN_POINT('Ctrl Pts',(-1.04178112698948,-3.07854306896254,
2.2661462876417));
#29017=CARTESIAN_POINT('Ctrl Pts',(2.01544067895206,-2.549654544323,2.42453901772905));
#29018=CARTESIAN_POINT('Ctrl Pts',(3.23589498051102,0.302857380478356,2.58293174781639));
#29019=CARTESIAN_POINT('Ctrl Pts',(1.50732273099005,2.87936039300554,2.74132447790374));
#29020=CARTESIAN_POINT('Ctrl Pts',(-1.5949449762732,2.83176433042226,2.89971720799108));
#29021=CARTESIAN_POINT('Ctrl Pts',(-3.24366282822075,0.203445412065843,
3.05810993807843));
#29022=CARTESIAN_POINT('Ctrl Pts',(-1.9362750553155,-2.61028300964445,3.21650266816577));
#29023=CARTESIAN_POINT('Ctrl Pts',(1.13573308688439,-3.04513528848185,3.37489539825311));
#29024=CARTESIAN_POINT('Ctrl Pts',(3.17269316854199,-0.704809622584737,
3.53328812834046));
#29025=CARTESIAN_POINT('Ctrl Pts',(2.31822570201349,2.27784286759623,3.69168085842781));
#29026=CARTESIAN_POINT('Ctrl Pts',(-0.648952098718329,3.18458784166478,
3.85007358851515));
#29027=CARTESIAN_POINT('Ctrl Pts',(-3.02470870901682,1.18906508190457,4.00846631860249));
#29028=CARTESIAN_POINT('Ctrl Pts',(-2.64390311385777,-1.89010974995907,
4.16685904868984));
#29029=CARTESIAN_POINT('Ctrl Pts',(0.146418271962415,-3.246736859336,4.32525177877718));
#29030=CARTESIAN_POINT('Ctrl Pts',(2.80330165993199,-1.64445685465812,4.48364450886452));
#29031=CARTESIAN_POINT('Ctrl Pts',(2.90540171220585,1.45649560042147,4.64203723895187));
#29032=CARTESIAN_POINT('Ctrl Pts',(0.359669751379629,3.23007371642187,4.80042996903921));
#29033=CARTESIAN_POINT('Ctrl Pts',(-2.5138465147678,2.05993064049482,4.95882269912656));
#29034=CARTESIAN_POINT('Ctrl Pts',(-3.09637381027549,-0.987526085984799,
5.1172154292139));
#29035=CARTESIAN_POINT('Ctrl Pts',(-0.857027054761158,-3.13500289806876,
5.27560815930125));
#29036=CARTESIAN_POINT('Ctrl Pts',(2.16336958524755,-2.4254011175679,5.43400088938859));
#29037=CARTESIAN_POINT('Ctrl Pts',(3.21218370019522,0.494585098517652,5.59239361947593));
#29038=CARTESIAN_POINT('Ctrl Pts',(1.33358065361335,2.96383217874895,5.75078634956329));
#29039=CARTESIAN_POINT('Ctrl Pts',(-1.76037844232411,2.73199675755249,5.90917907965061));
#29040=CARTESIAN_POINT('Ctrl Pts',(-3.25002018164994,0.0103615802535554,
6.06757180973798));
#29041=CARTESIAN_POINT('Ctrl Pts',(-1.77776255808964,-2.72071660239216,
6.2259645398253));
#29042=CARTESIAN_POINT('Ctrl Pts',(1.3146554010584,-2.97227517567693,6.38435726991266));
#29043=CARTESIAN_POINT('Ctrl Pts',(3.20896480174417,-0.515056739247718,
6.54275));
#29044=CARTESIAN_POINT('Ctrl Pts',(2.1787905775359,2.41155762168733,6.70114273008734));
#29045=CARTESIAN_POINT('Ctrl Pts',(-0.837020062071456,3.14040378919134,
6.85953546017469));
#29046=CARTESIAN_POINT('Ctrl Pts',(-3.09001414977857,1.00724927284447,7.01792819026203));
#29047=CARTESIAN_POINT('Ctrl Pts',(-2.52693005027509,-2.04385984463079,
7.17632092034938));
#29048=CARTESIAN_POINT('Ctrl Pts',(0.339066673656528,-3.23230139904882,
7.33471365043672));
#29049=CARTESIAN_POINT('Ctrl Pts',(2.8960556657748,-1.47499156750509,7.49310638052407));
#29050=CARTESIAN_POINT('Ctrl Pts',(2.81373014539465,1.62654886565846,7.6514991106114));
#29051=CARTESIAN_POINT('Ctrl Pts',(0.167117310113194,3.24573725802598,7.80989184069877));
#29052=CARTESIAN_POINT('Ctrl Pts',(-2.63179754998223,1.90692952134707,7.96828457078609));
#29053=CARTESIAN_POINT('Ctrl Pts',(-3.03222900048216,-1.16975460337304,
8.12667730087346));
#29054=CARTESIAN_POINT('Ctrl Pts',(-0.669244643485845,-3.18038522047927,
8.28507003096078));
#29055=CARTESIAN_POINT('Ctrl Pts',(2.30365447476264,-2.2925781566576,8.44346276104813));
#29056=CARTESIAN_POINT('Ctrl Pts',(3.17712271574022,0.68456540418354,8.60185549113548));
#29057=CARTESIAN_POINT('Ctrl Pts',(1.15512655292908,3.03783165929181,8.76024822122282));
#29058=CARTESIAN_POINT('Ctrl Pts',(-1.91959187311326,2.62257613505404,8.91864095131017));
#29059=CARTESIAN_POINT('Ctrl Pts',(-3.24489410227238,-0.182758880811296,
9.0770336813975));
#29060=CARTESIAN_POINT('Ctrl Pts',(-1.61296861068713,-2.82153695783264,
9.23542641148485));
#29061=CARTESIAN_POINT('Ctrl Pts',(1.48893258361032,-2.8889129971221,9.3938191415722));
#29062=CARTESIAN_POINT('Ctrl Pts',(3.23389805926952,-0.323483980639333,
9.55221187165954));
#29063=CARTESIAN_POINT('Ctrl Pts',(2.03165703588272,2.53675151168294,9.71060460174689));
#29064=CARTESIAN_POINT('Ctrl Pts',(-1.02213054532559,3.08512361045549,9.86899733183423));
#29065=CARTESIAN_POINT('Ctrl Pts',(-3.14440150762802,0.821874505203878,
10.0273900619216));
#29066=CARTESIAN_POINT('Ctrl Pts',(-2.40102847341415,-2.19038827912587,
10.1857827920089));
#29067=CARTESIAN_POINT('Ctrl Pts',(0.530517036106232,-3.2064451060136,10.3441755220963));
#29068=CARTESIAN_POINT('Ctrl Pts',(2.97857691064031,-1.30031462764898,10.5025682521836));
#29069=CARTESIAN_POINT('Ctrl Pts',(2.71211670196235,1.79085497414346,10.660960982271));
#29070=CARTESIAN_POINT('Ctrl Pts',(-0.0260256140978684,3.24993249328171,
10.8193537123583));
#29071=CARTESIAN_POINT('Ctrl Pts',(-2.74044953903841,1.74719056415196,10.9777464424457));
#29072=CARTESIAN_POINT('Ctrl Pts',(-2.95737028245133,-1.34784997531299,
11.136139172533));
#29073=CARTESIAN_POINT('Ctrl Pts',(-0.479097560645698,-3.21453014776045,
11.2945319026203));
#29074=CARTESIAN_POINT('Ctrl Pts',(2.43579976049286,-2.15165472840333,11.4529246327077));
#29075=CARTESIAN_POINT('Ctrl Pts',(3.13083586370518,0.872126904764919,11.611317362795));
#29076=CARTESIAN_POINT('Ctrl Pts',(0.972590992735389,3.10109743547788,11.7697100928824));
#29077=CARTESIAN_POINT('Ctrl Pts',(-2.07202272541781,2.50388904882577,11.9281028229697));
#29078=CARTESIAN_POINT('Ctrl Pts',(-3.22830269569097,-0.375233591875627,
12.0864955530571));
#29079=CARTESIAN_POINT('Ctrl Pts',(-1.44247549027371,-2.91238785250816,
12.2448882831444));
#29080=CARTESIAN_POINT('Ctrl Pts',(1.65794885510707,-2.79534329507605,12.4032810132317));
#29081=CARTESIAN_POINT('Ctrl Pts',(3.24740484239397,-0.1307682418392,12.5616737433191));
#29082=CARTESIAN_POINT('Ctrl Pts',(1.87734495097103,2.65298218586953,12.7200664734064));
#29083=CARTESIAN_POINT('Ctrl Pts',(-1.20362948971966,3.0189426286292,12.8784592034938));
#29084=CARTESIAN_POINT('Ctrl Pts',(-3.18767861318299,0.633595772187016,
13.0368519335811));
#29085=CARTESIAN_POINT('Ctrl Pts',(-2.26664323693112,-2.32917731827181,
13.1952446636685));
#29086=CARTESIAN_POINT('Ctrl Pts',(0.720092899353666,-3.16925933930592,
13.3536373937558));
#29087=CARTESIAN_POINT('Ctrl Pts',(3.05057381856114,-1.12104322886633,13.5120301238432));
#29088=CARTESIAN_POINT('Ctrl Pts',(2.60092041717278,1.94883337589723,13.6704228539305));
#29089=CARTESIAN_POINT('Ctrl Pts',(-0.219076580860588,3.24264459896475,
13.8288155840179));
#29090=CARTESIAN_POINT('Ctrl Pts',(-2.83941857707695,1.58127818160812,13.9872083141052));
#29091=CARTESIAN_POINT('Ctrl Pts',(-2.87206215778837,-1.52118292958987,
14.1456010441925));
#29092=CARTESIAN_POINT('Ctrl Pts',(-0.287257661300916,-3.23731703413455,
14.3039937742799));
#29093=CARTESIAN_POINT('Ctrl Pts',(2.55933852768325,-2.00312876376139,14.4623865043672));
#29094=CARTESIAN_POINT('Ctrl Pts',(3.07348669145905,1.05660688095643,14.6207792344546));
#29095=CARTESIAN_POINT('Ctrl Pts',(0.786618933970887,3.15340596754972,14.7791719645419));
#29096=CARTESIAN_POINT('Ctrl Pts',(-2.2171324086089,2.37635486118404,14.9375646946292));
#29097=CARTESIAN_POINT('Ctrl Pts',(-3.20030458502806,-0.566382473584868,
15.0959574247166));
#29098=CARTESIAN_POINT('Ctrl Pts',(-1.26688560774635,-2.99294827892075,
15.2543501548039));
#29099=CARTESIAN_POINT('Ctrl Pts',(1.82110702300624,-2.69189668354728,15.4127428848913));
#29100=CARTESIAN_POINT('Ctrl Pts',(3.24943742683135,0.0624095462628093,
15.5711356149786));
#29101=CARTESIAN_POINT('Ctrl Pts',(1.7163995608183,2.75983896106814,15.729528345066));
#29102=CARTESIAN_POINT('Ctrl Pts',(-1.38087559767885,2.94209468431,15.8879210751533));
#29103=CARTESIAN_POINT('Ctrl Pts',(-3.21969255232482,0.443078326528232,
16.0463138052407));
#29104=CARTESIAN_POINT('Ctrl Pts',(-2.12424917242148,-2.45973657111239,
16.204706535328));
#29105=CARTESIAN_POINT('Ctrl Pts',(0.907124431089416,-3.12087549196088,
16.3630992654154));
#29106=CARTESIAN_POINT('Ctrl Pts',(3.11179199122249,-0.937810793091581,
16.5214919955027));
#29107=CARTESIAN_POINT('Ctrl Pts',(2.48053420193034,2.09992586819762,16.6798847255901));
#29108=CARTESIAN_POINT('Ctrl Pts',(-0.411353505584467,3.2238993461078,16.8382774556774));
#29109=CARTESIAN_POINT('Ctrl Pts',(-2.92835491344629,1.40977856029352,16.9966701857647));
#29110=CARTESIAN_POINT('Ctrl Pts',(-2.77660616210399,-1.68914094686405,
17.1550629158521));
#29111=CARTESIAN_POINT('Ctrl Pts',(-0.0944025666701746,-3.24866550773817,
17.3134556459394));
#29112=CARTESIAN_POINT('Ctrl Pts',(2.67383386050354,-1.84752478479548,17.4718483760268));
#29113=CARTESIAN_POINT('Ctrl Pts',(3.00527861799256,1.23735298349299,17.6302411061141));
#29114=CARTESIAN_POINT('Ctrl Pts',(0.597865981467751,3.19457342078244,17.7886338362015));
#29115=CARTESIAN_POINT('Ctrl Pts',(-2.35440533867421,2.24042230497867,17.9470265662888));
#29116=CARTESIAN_POINT('Ctrl Pts',(-3.16100416204722,-0.75552652313063,
18.1054192963761));
#29117=CARTESIAN_POINT('Ctrl Pts',(-1.08680894633521,-3.06294047971977,
18.2638120264635));
#29118=CARTESIAN_POINT('Ctrl Pts',(1.97781066311423,-2.57892551637815,18.4222047565508));
#29119=CARTESIAN_POINT('Ctrl Pts',(3.24002669195714,0.255341690782801,18.5805974866382));
#29120=CARTESIAN_POINT('Ctrl Pts',(1.54931685428281,2.85699226584485,18.7389902167255));
#29121=CARTESIAN_POINT('Ctrl Pts',(-1.55310378277979,2.85475965565781,18.8973829468129));
#29122=CARTESIAN_POINT('Ctrl Pts',(-3.24059534293408,0.251170398141146,
19.0557756769002));
#29123=CARTESIAN_POINT('Ctrl Pts',(-1.97384274968036,-2.58193937867803,
19.2141684069875));
#29124=CARTESIAN_POINT('Ctrl Pts',(1.08998032784309,-3.06082255890563,19.3725611370749));
#29125=CARTESIAN_POINT('Ctrl Pts',(3.16389391825703,-0.752516084320418,
19.5309538671622));
#29126=CARTESIAN_POINT('Ctrl Pts',(2.34757039202943,2.24621112130266,19.6893465972496));
#29127=CARTESIAN_POINT('Ctrl Pts',(0.38722186627484,2.87341499502444,19.7949417506411));
#29128=CARTESIAN_POINT('Ctrl Pts',(-0.509883685250381,2.70426773226936,
19.8477393273369));
#29129=CARTESIAN_POINT('Ctrl Pts',(-1.28892185405322,2.64462557919718,0.));
#29130=CARTESIAN_POINT('Ctrl Pts',(-2.16624189914077,2.21704256404099,0.0527975766957814));
#29131=CARTESIAN_POINT('Ctrl Pts',(-3.44706110523448,0.427824646218769,
0.158392730087344));
#29132=CARTESIAN_POINT('Ctrl Pts',(-2.23297934450677,-2.66493400478364,
0.316785460174689));
#29133=CARTESIAN_POINT('Ctrl Pts',(1.01903298359751,-3.32069221456353,0.475178190262033));
#29134=CARTESIAN_POINT('Ctrl Pts',(3.34085837172009,-0.954300736940341,
0.633570920349377));
#29135=CARTESIAN_POINT('Ctrl Pts',(2.61877776038273,2.28394466972569,0.791963650436721));
#29136=CARTESIAN_POINT('Ctrl Pts',(-0.490328006709216,3.43959640275791,
0.950356380524067));
#29137=CARTESIAN_POINT('Ctrl Pts',(-3.15236109266777,1.46116781824645,1.10874911061141));
#29138=CARTESIAN_POINT('Ctrl Pts',(-2.94160788454626,-1.84920148739755,
1.26714184069876));
#29139=CARTESIAN_POINT('Ctrl Pts',(-0.0499677750165847,-3.47414326454672,
1.4255345707861));
#29140=CARTESIAN_POINT('Ctrl Pts',(2.88717975101212,-1.93301610795034,1.58392730087344));
#29141=CARTESIAN_POINT('Ctrl Pts',(3.19311784272742,1.36980566874669,1.74232003096079));
#29142=CARTESIAN_POINT('Ctrl Pts',(0.589006009320745,3.42423461791024,1.90071276104813));
#29143=CARTESIAN_POINT('Ctrl Pts',(-2.55189087162783,2.35800636743253,2.05910549113548));
#29144=CARTESIAN_POINT('Ctrl Pts',(-3.3671294354981,-0.857192605315573,
2.21749822122282));
#29145=CARTESIAN_POINT('Ctrl Pts',(-1.11374014799495,-3.29118749073838,
2.37589095131016));
#29146=CARTESIAN_POINT('Ctrl Pts',(2.15465335462323,-2.72576701186384,2.53428368139751));
#29147=CARTESIAN_POINT('Ctrl Pts',(3.45940818193263,0.323776669606257,2.69267641148485));
#29148=CARTESIAN_POINT('Ctrl Pts',(1.61143813992893,3.07824665580557,2.8510691415722));
#29149=CARTESIAN_POINT('Ctrl Pts',(-1.70511272271897,3.02736298704623,3.00946187165954));
#29150=CARTESIAN_POINT('Ctrl Pts',(-3.46771257873317,0.21749801131251,3.16785460174689));
#29151=CARTESIAN_POINT('Ctrl Pts',(-2.07001951830114,-2.79058327143165,
3.32624733183423));
#29152=CARTESIAN_POINT('Ctrl Pts',(1.214181658219,-3.2554721322885,3.48464006192158));
#29153=CARTESIAN_POINT('Ctrl Pts',(3.39184082676336,-0.753492987182631,
3.64303279200892));
#29154=CARTESIAN_POINT('Ctrl Pts',(2.47835266886366,2.4351804680864,3.80142552209627));
#29155=CARTESIAN_POINT('Ctrl Pts',(-0.693777212644261,3.40455710147877,
3.9598182521836));
#29156=CARTESIAN_POINT('Ctrl Pts',(-3.23363462626441,1.27119745787964,4.11821098227095));
#29157=CARTESIAN_POINT('Ctrl Pts',(-2.82652561946628,-2.02066543356311,
4.2766037123583));
#29158=CARTESIAN_POINT('Ctrl Pts',(0.156531831552572,-3.4709989426157,4.43499644244564));
#29159=CARTESIAN_POINT('Ctrl Pts',(2.9969343125167,-1.75804453855951,4.59338917253298));
#29160=CARTESIAN_POINT('Ctrl Pts',(3.10608672887731,1.55710022339821,4.75178190262033));
#29161=CARTESIAN_POINT('Ctrl Pts',(0.384513245395842,3.4531848252599,4.91017463270768));
#29162=CARTESIAN_POINT('Ctrl Pts',(-2.68748561176641,2.20221637440662,5.06856736279502));
#29163=CARTESIAN_POINT('Ctrl Pts',(-3.31024985609926,-1.05573754472964,
5.22696009288236));
#29164=CARTESIAN_POINT('Ctrl Pts',(-0.916224544750279,-3.35154717358869,
5.38535282296971));
#29165=CARTESIAN_POINT('Ctrl Pts',(2.31280016466036,-2.59293101942941,5.54374555305705));
#29166=CARTESIAN_POINT('Ctrl Pts',(3.43405909068504,0.528747609789137,5.70213828314441));
#29167=CARTESIAN_POINT('Ctrl Pts',(1.42569516383024,3.16855316714268,5.86053101323173));
#29168=CARTESIAN_POINT('Ctrl Pts',(-1.88197318619781,2.92070416160353,6.01892374331909));
#29169=CARTESIAN_POINT('Ctrl Pts',(-3.47450905408259,0.01107728641468,6.17731647340643));
#29170=CARTESIAN_POINT('Ctrl Pts',(-1.90055807621346,-2.90864485149298,
6.33570920349377));
#29171=CARTESIAN_POINT('Ctrl Pts',(1.40546268597539,-3.17757934779089,6.49410193358112));
#29172=CARTESIAN_POINT('Ctrl Pts',(3.43061785303504,-0.550633289598217,
6.65249466366846));
#29173=CARTESIAN_POINT('Ctrl Pts',(2.32928633223293,2.57813131078488,6.81088739375581));
#29174=CARTESIAN_POINT('Ctrl Pts',(-0.894835607648314,3.35732112084339,
6.96928012384315));
#29175=CARTESIAN_POINT('Ctrl Pts',(-3.30345091432585,1.07682307266153,7.1276728539305));
#29176=CARTESIAN_POINT('Ctrl Pts',(-2.70147286724138,-2.18503551933032,
7.28606558401784));
#29177=CARTESIAN_POINT('Ctrl Pts',(0.362487049837071,-3.45556638076552,
7.44445831410518));
#29178=CARTESIAN_POINT('Ctrl Pts',(3.09609512232424,-1.5768737637162,7.60285104419254));
#29179=CARTESIAN_POINT('Ctrl Pts',(3.00808312548869,1.738899589777,7.76124377427986));
#29180=CARTESIAN_POINT('Ctrl Pts',(0.178660615820388,3.46993029577413,7.91963650436722));
#29181=CARTESIAN_POINT('Ctrl Pts',(-2.81358388712632,2.03864699820239,8.07802923445455));
#29182=CARTESIAN_POINT('Ctrl Pts',(-3.2416743673507,-1.25055314530725,8.23642196454191));
#29183=CARTESIAN_POINT('Ctrl Pts',(-0.71547142578278,-3.40006419234473,
8.39481469462925));
#29184=CARTESIAN_POINT('Ctrl Pts',(2.46277496220876,-2.45093356880478,8.5532074247166));
#29185=CARTESIAN_POINT('Ctrl Pts',(3.39657633638654,0.731850438460929,8.71160015480394));
#29186=CARTESIAN_POINT('Ctrl Pts',(1.23491469050688,3.24766401900608,8.86999288489128));
#29187=CARTESIAN_POINT('Ctrl Pts',(-2.05218397748206,2.80372552075669,9.02838561497863));
#29188=CARTESIAN_POINT('Ctrl Pts',(-3.46902890066391,-0.195382597830646,
9.18677834506597));
#29189=CARTESIAN_POINT('Ctrl Pts',(-1.72438130489958,-3.01642917843089,
9.34517107515332));
#29190=CARTESIAN_POINT('Ctrl Pts',(1.59177772860667,-3.08845908761769,9.50356380524066));
#29191=CARTESIAN_POINT('Ctrl Pts',(3.45727332720986,-0.345828012369911,
9.66195653532801));
#29192=CARTESIAN_POINT('Ctrl Pts',(2.17198982511594,2.71197272714333,9.82034926541533));
#29193=CARTESIAN_POINT('Ctrl Pts',(-1.09273224032263,3.29822257043638,9.97874199550271));
#29194=CARTESIAN_POINT('Ctrl Pts',(-3.36159497396661,0.878643900666754,
10.13713472559));
#29195=CARTESIAN_POINT('Ctrl Pts',(-2.56687488191302,-2.34168512267993,
10.2955274556774));
#29196=CARTESIAN_POINT('Ctrl Pts',(0.567161476628229,-3.42792411418417,
10.4539201857647));
#29197=CARTESIAN_POINT('Ctrl Pts',(3.1843163629363,-1.39013135131635,10.6123129158521));
#29198=CARTESIAN_POINT('Ctrl Pts',(2.89945092953635,1.91455482564153,10.7707056459394));
#29199=CARTESIAN_POINT('Ctrl Pts',(-0.0278232831696277,3.47441530880954,
10.9290983760268));
#29200=CARTESIAN_POINT('Ctrl Pts',(-2.92974080265911,1.86787438078978,11.0874911061141));
#29201=CARTESIAN_POINT('Ctrl Pts',(-3.16164492782793,-1.44095011139053,
11.2458838362014));
#29202=CARTESIAN_POINT('Ctrl Pts',(-0.512190300125254,-3.43656761458786,
11.4042765662888));
#29203=CARTESIAN_POINT('Ctrl Pts',(2.60404792854797,-2.300276126686,11.5626692963761));
#29204=CARTESIAN_POINT('Ctrl Pts',(3.34709230936765,0.932367387754601,11.7210620264635));
#29205=CARTESIAN_POINT('Ctrl Pts',(1.03977083873454,3.31529975659725,11.8794547565508));
#29206=CARTESIAN_POINT('Ctrl Pts',(-2.21514369676135,2.67684035307953,12.0378474866382));
#29207=CARTESIAN_POINT('Ctrl Pts',(-3.45129147468958,-0.401152128140284,
12.1962402167255));
#29208=CARTESIAN_POINT('Ctrl Pts',(-1.54211170119684,-3.11355542333973,
12.3546329468129));
#29209=CARTESIAN_POINT('Ctrl Pts',(1.77246847290372,-2.98842623896573,12.5130256769002));
#29210=CARTESIAN_POINT('Ctrl Pts',(3.47171306531437,-0.139800805798732,
12.6714184069876));
#29211=CARTESIAN_POINT('Ctrl Pts',(2.00701893071743,2.8362318108572,12.8298111370749));
#29212=CARTESIAN_POINT('Ctrl Pts',(-1.28676787405936,3.22747026500092,12.9882038671622));
#29213=CARTESIAN_POINT('Ctrl Pts',(-3.40786136207529,0.67736017749117,13.1465965972496));
#29214=CARTESIAN_POINT('Ctrl Pts',(-2.42320724454521,-2.4900607468815,13.3049893273369));
#29215=CARTESIAN_POINT('Ctrl Pts',(0.769831926801966,-3.38816981239912,
13.4633820574243));
#29216=CARTESIAN_POINT('Ctrl Pts',(3.2612863183382,-1.19847712660562,13.6217747875116));
#29217=CARTESIAN_POINT('Ctrl Pts',(2.78057397595216,2.08344528064305,13.780167517599));
#29218=CARTESIAN_POINT('Ctrl Pts',(-0.234208872928009,3.4666240172562,13.9385602476863));
#29219=CARTESIAN_POINT('Ctrl Pts',(-3.03554593601806,1.69050192058546,14.0969529777737));
#29220=CARTESIAN_POINT('Ctrl Pts',(-3.0704443090743,-1.62625570500076,14.255345707861));
#29221=CARTESIAN_POINT('Ctrl Pts',(-0.307099429929689,-3.46092846116604,
14.4137384379484));
#29222=CARTESIAN_POINT('Ctrl Pts',(2.73611989768734,-2.14149101764928,14.5721311680357));
#29223=CARTESIAN_POINT('Ctrl Pts',(3.28578185371621,1.12958996230764,14.730523898123));
#29224=CARTESIAN_POINT('Ctrl Pts',(0.84095311888407,3.37122139958136,14.8889166282103));
#29225=CARTESIAN_POINT('Ctrl Pts',(-2.37027655129843,2.54049698753116,15.0473093582977));
#29226=CARTESIAN_POINT('Ctrl Pts',(-3.42135944856103,-0.605504249990604,
15.2057020883851));
#29227=CARTESIAN_POINT('Ctrl Pts',(-1.35439328637246,-3.19968040574805,
15.3640948184724));
#29228=CARTESIAN_POINT('Ctrl Pts',(1.94689647640166,-2.87783425236815,15.5224875485598));
#29229=CARTESIAN_POINT('Ctrl Pts',(3.47388604659947,0.0667203652382213,
15.6808802786471));
#29230=CARTESIAN_POINT('Ctrl Pts',(1.83495654831874,2.95046951159947,15.8392730087344));
#29231=CARTESIAN_POINT('Ctrl Pts',(-1.47625691489125,3.14531419722255,15.9976657388218));
#29232=CARTESIAN_POINT('Ctrl Pts',(-3.44208660228554,0.473683106918002,
16.1560584689091));
#29233=CARTESIAN_POINT('Ctrl Pts',(-2.27097758480962,-2.62963812816981,
16.3144511989965));
#29234=CARTESIAN_POINT('Ctrl Pts',(0.96978230067469,-3.33644394416579,16.4728439290838));
#29235=CARTESIAN_POINT('Ctrl Pts',(3.32673301814246,-1.00258826391623,16.6312366591711));
#29236=CARTESIAN_POINT('Ctrl Pts',(2.65187231520301,2.24497419528354,16.7896293892585));
#29237=CARTESIAN_POINT('Ctrl Pts',(-0.4397669551874,3.44658397223117,16.9480221193458));
#29238=CARTESIAN_POINT('Ctrl Pts',(-3.13062537820028,1.50715629387405,17.1064148494332));
#29239=CARTESIAN_POINT('Ctrl Pts',(-2.96839487469096,-1.80581509820695,
17.2648075795206));
#29240=CARTESIAN_POINT('Ctrl Pts',(-0.10092324179282,-3.47306080868451,
17.4232003096079));
#29241=CARTESIAN_POINT('Ctrl Pts',(2.85852377467875,-1.97513899410775,17.5815930396952));
#29242=CARTESIAN_POINT('Ctrl Pts',(3.21286243919721,1.32282075308833,17.7399857697826));
#29243=CARTESIAN_POINT('Ctrl Pts',(0.639162420426306,3.41523241520465,17.8983784998699));
#29244=CARTESIAN_POINT('Ctrl Pts',(-2.51703134411028,2.3951751523171,18.0567712299573));
#29245=CARTESIAN_POINT('Ctrl Pts',(-3.37934442470143,-0.807713059764507,
18.2151639600446));
#29246=CARTESIAN_POINT('Ctrl Pts',(-1.16187817707109,-3.27450718275222,
18.3735566901319));
#29247=CARTESIAN_POINT('Ctrl Pts',(2.11442411805664,-2.75705981982905,18.5319494202193));
#29248=CARTESIAN_POINT('Ctrl Pts',(3.46382528337386,0.272978925336754,18.6903421503066));
#29249=CARTESIAN_POINT('Ctrl Pts',(1.65633292625143,3.05433349342538,18.848734880394));
#29250=CARTESIAN_POINT('Ctrl Pts',(-1.66038142952661,3.05194666999799,19.0071276104813));
#29251=CARTESIAN_POINT('Ctrl Pts',(-3.4644332128197,0.268519508705312,19.1655203405687));
#29252=CARTESIAN_POINT('Ctrl Pts',(-2.11018212865929,-2.76028185885138,
19.323913070656));
#29253=CARTESIAN_POINT('Ctrl Pts',(1.16526861563674,-3.27224297064484,19.4823058007433));
#29254=CARTESIAN_POINT('Ctrl Pts',(3.38243378524502,-0.804494680702798,
19.6406985308307));
#29255=CARTESIAN_POINT('Ctrl Pts',(2.50972428671554,2.40136381995787,19.799091260918));
#29256=CARTESIAN_POINT('Ctrl Pts',(0.413968469459689,3.07189059093186,19.9046864143096));
#29257=CARTESIAN_POINT('Ctrl Pts',(-0.545102916878511,2.8910598074081,19.9574839910054));
#29258=CARTESIAN_POINT('Ctrl Pts',(-2.94191884508495,-0.00265442804262754,
18.1778238829104));
#29259=CARTESIAN_POINT('Ctrl Pts',(-2.94401095921365,-0.232682134900822,
18.1902705752885));
#29260=CARTESIAN_POINT('Ctrl Pts',(-2.91929265776683,-0.462265462611949,
18.2027172676665));
#29261=CARTESIAN_POINT('Ctrl Pts',(-2.86604786999785,-0.685030711582192,
18.2151639600446));
#29262=CARTESIAN_POINT('Ctrl Pts',(-2.64018900882465,-1.62997776742708,
18.2679615367404));
#29263=CARTESIAN_POINT('Ctrl Pts',(-1.90103359294787,-2.45224247508964,
18.3207591134362));
#29264=CARTESIAN_POINT('Ctrl Pts',(-0.985405502488203,-2.77713360176707,
18.3735566901319));
#29265=CARTESIAN_POINT('Ctrl Pts',(-0.0697774120285166,-3.1020247284445,
18.4263542668277));
#29266=CARTESIAN_POINT('Ctrl Pts',(1.02232335301407,-2.92954227413678,18.4791518435235));
#29267=CARTESIAN_POINT('Ctrl Pts',(1.7932739297549,-2.33829458945527,18.5319494202193));
#29268=CARTESIAN_POINT('Ctrl Pts',(2.56422450649571,-1.74704690477378,18.5847469969151));
#29269=CARTESIAN_POINT('Ctrl Pts',(3.01402489493477,-0.737033989718538,
18.6375445736108));
#29270=CARTESIAN_POINT('Ctrl Pts',(2.93767636296726,0.231531562490516,18.6903421503066));
#29271=CARTESIAN_POINT('Ctrl Pts',(2.86132783099973,1.2000971146996,18.7431397270024));
#29272=CARTESIAN_POINT('Ctrl Pts',(2.25883037862559,2.12721530406249,18.7959373036982));
#29273=CARTESIAN_POINT('Ctrl Pts',(1.40479592647551,2.59037659483937,18.848734880394));
#29274=CARTESIAN_POINT('Ctrl Pts',(0.550761474325412,3.05353788561626,18.9015324570898));
#29275=CARTESIAN_POINT('Ctrl Pts',(-0.554809977600626,3.05274227780712,
18.9543300337855));
#29276=CARTESIAN_POINT('Ctrl Pts',(-1.40827100077916,2.58843994702042,19.0071276104813));
#29277=CARTESIAN_POINT('Ctrl Pts',(-1.68238460173924,2.4393158741341,19.0240850736542));
#29278=CARTESIAN_POINT('Ctrl Pts',(-1.93049154169819,2.24237837966061,19.0410425368271));
#29279=CARTESIAN_POINT('Ctrl Pts',(-2.14350474087479,2.01162918712774,19.058));
#29280=CARTESIAN_POINT('Ctrl Pts',(-1.37997554054989,-1.93359434039964,
5.03069808033274E-17));
#29281=CARTESIAN_POINT('Ctrl Pts',(-1.43480608311011,-1.90379100615021,
4.05392308728466E-17));
#29282=CARTESIAN_POINT('Ctrl Pts',(-1.48827102383981,-1.87175009325149,
-2.56174624183488E-16));
#29283=CARTESIAN_POINT('Ctrl Pts',(-1.54021573000326,-1.83750293771675,
-2.32452945780892E-16));
#29284=CARTESIAN_POINT('Ctrl Pts',(-1.60834066683741,-1.79258815274882,
-2.34206640027434E-16));
#29285=CARTESIAN_POINT('Ctrl Pts',(-1.67385212815421,-1.74388071234801,
2.35502939941775E-16));
#29286=CARTESIAN_POINT('Ctrl Pts',(-1.7366654506395,-1.6917391145835,2.60208521396521E-16));
#29287=CARTESIAN_POINT('Ctrl Pts',(-1.77318557553109,-1.66142360846054,
2.74572527065185E-16));
#29288=CARTESIAN_POINT('Ctrl Pts',(-1.80879333390789,-1.62994627115077,
-1.27188329331984E-16));
#29289=CARTESIAN_POINT('Ctrl Pts',(-1.84346892862395,-1.59737031707875,
-1.73472347597681E-16));
#29290=CARTESIAN_POINT('Ctrl Pts',(-1.85655816608735,-1.58507364554545,
-1.90943497286695E-16));
#29291=CARTESIAN_POINT('Ctrl Pts',(-1.86951455362061,-1.57262038350302,
-1.1893963212715E-16));
#29292=CARTESIAN_POINT('Ctrl Pts',(-1.8823369229035,-1.56001375633204,-1.66533453693773E-16));
#29293=CARTESIAN_POINT('Ctrl Pts',(-1.89389529438543,-1.54864985963231,
-2.09435592742768E-16));
#29294=CARTESIAN_POINT('Ctrl Pts',(-1.90534102035706,-1.53716495022738,
3.49299600923418E-16));
#29295=CARTESIAN_POINT('Ctrl Pts',(-1.9166678489872,-1.52556749612954,3.05311331771918E-16));
#29296=CARTESIAN_POINT('Ctrl Pts',(-1.97639856958762,-1.46440966342857,
7.33442825493013E-17));
#29297=CARTESIAN_POINT('Ctrl Pts',(-2.03287303298855,-1.40007886819707,
-7.0183037565297E-16));
#29298=CARTESIAN_POINT('Ctrl Pts',(-2.08599777480493,-1.33296674038781,
-4.44089209850063E-16));
#29299=CARTESIAN_POINT('Ctrl Pts',(-2.13221332454416,-1.274582948301,-2.19868832287029E-16));
#29300=CARTESIAN_POINT('Ctrl Pts',(-2.17589371235756,-1.21409310252408,
-1.30713211170112E-16));
#29301=CARTESIAN_POINT('Ctrl Pts',(-2.21696145780543,-1.1517270622244,-1.2490009027033E-16));
#29302=CARTESIAN_POINT('Ctrl Pts',(-2.23761972751426,-1.12035513111075,
-1.21975921483168E-16));
#29303=CARTESIAN_POINT('Ctrl Pts',(-2.257616638896,-1.08850807754864,-6.50635459664472E-19));
#29304=CARTESIAN_POINT('Ctrl Pts',(-2.27694058302463,-1.05621312605931,
2.77555756156289E-17));
#29305=CARTESIAN_POINT('Ctrl Pts',(-2.28638312411741,-1.04043237216676,
4.16361174751555E-17));
#29306=CARTESIAN_POINT('Ctrl Pts',(-2.29566596401088,-1.0245426554578,-3.86134059335254E-16));
#29307=CARTESIAN_POINT('Ctrl Pts',(-2.30477629260578,-1.00856764802397,
-3.60822483003176E-16));
#29308=CARTESIAN_POINT('Ctrl Pts',(-2.34868382122166,-0.931575573728042,
-2.38832507500552E-16));
#29309=CARTESIAN_POINT('Ctrl Pts',(-2.38864775623492,-0.852506148187216,
7.6589648086775E-17));
#29310=CARTESIAN_POINT('Ctrl Pts',(-2.42457139730333,-0.771756361747471,
1.11022302462516E-16));
#29311=CARTESIAN_POINT('Ctrl Pts',(-2.46298089184026,-0.685418830559891,
1.47837636621387E-16));
#29312=CARTESIAN_POINT('Ctrl Pts',(-2.496772671788,-0.597159876911868,-2.6411927253517E-16));
#29313=CARTESIAN_POINT('Ctrl Pts',(-2.52578830996096,-0.5074153351261,-2.22044604925031E-16));
#29314=CARTESIAN_POINT('Ctrl Pts',(-2.54755003859068,-0.440106928786774,
-1.90488604217428E-16));
#29315=CARTESIAN_POINT('Ctrl Pts',(-2.56662441067748,-0.371961718591897,
-1.06288902356375E-16));
#29316=CARTESIAN_POINT('Ctrl Pts',(-2.58292557654155,-0.303150270529533,
-1.11022302462516E-16));
#29317=CARTESIAN_POINT('Ctrl Pts',(-2.5951514509396,-0.251541684482761,
-1.14572352542121E-16));
#29318=CARTESIAN_POINT('Ctrl Pts',(-2.60581707499254,-0.199558087757334,
-1.32861127945469E-16));
#29319=CARTESIAN_POINT('Ctrl Pts',(-2.61487919945664,-0.147268754493998,
-1.38777878078145E-16));
#29320=CARTESIAN_POINT('Ctrl Pts',(-2.61743940316675,-0.132496131854521,
-1.4044946024428E-16));
#29321=CARTESIAN_POINT('Ctrl Pts',(-2.61987158272419,-0.117699096439989,
-1.07679138130245E-16));
#29322=CARTESIAN_POINT('Ctrl Pts',(-2.62217466731863,-0.102879189619736,
-1.11022302462516E-16));
#29323=CARTESIAN_POINT('Ctrl Pts',(-2.62424692676471,-0.089544598275464,
-1.14030400334403E-16));
#29324=CARTESIAN_POINT('Ctrl Pts',(-2.62621322332593,-0.0762007531359675,
9.91403158685596E-17));
#29325=CARTESIAN_POINT('Ctrl Pts',(-2.62807300875564,-0.0628502760411497,
1.11022302462516E-16));
#29326=CARTESIAN_POINT('Ctrl Pts',(-2.64084702393496,0.0288480426655374,
1.92634231820763E-16));
#29327=CARTESIAN_POINT('Ctrl Pts',(-2.64860284780981,0.120877572624176,
2.34034299737326E-18));
#29328=CARTESIAN_POINT('Ctrl Pts',(-2.65120733482282,0.212843544851723,
-5.55111512312578E-17));
#29329=CARTESIAN_POINT('Ctrl Pts',(-2.65227730220756,0.250624724138807,
-7.92775250599356E-17));
#29330=CARTESIAN_POINT('Ctrl Pts',(-2.65247737800954,0.28839553131628,1.67382252759083E-16));
#29331=CARTESIAN_POINT('Ctrl Pts',(-2.65179610762442,0.326129846634779,
1.66533453693773E-16));
#29332=CARTESIAN_POINT('Ctrl Pts',(-2.65019510065319,0.41480668214537,1.65536101357303E-16));
#29333=CARTESIAN_POINT('Ctrl Pts',(-2.64373047396203,0.503281469119527,
3.1574695155968E-17));
#29334=CARTESIAN_POINT('Ctrl Pts',(-2.63264650872894,0.591292908473233,
5.55111512312578E-17));
#29335=CARTESIAN_POINT('Ctrl Pts',(-2.62134112159331,0.681062532730685,
7.99257805534553E-17));
#29336=CARTESIAN_POINT('Ctrl Pts',(-2.60522989313478,0.770350844351005,
-2.70863134523007E-16));
#29337=CARTESIAN_POINT('Ctrl Pts',(-2.58451809222978,0.858883818120269,
-4.16333634234434E-16));
#29338=CARTESIAN_POINT('Ctrl Pts',(-2.57994896726511,0.878414626788261,
-4.48425140661245E-16));
#29339=CARTESIAN_POINT('Ctrl Pts',(-2.57515574764109,0.897908663068738,
2.12915568004684E-16));
#29340=CARTESIAN_POINT('Ctrl Pts',(-2.57014030159083,0.917362948618063,
1.94289029309402E-16));
#29341=CARTESIAN_POINT('Ctrl Pts',(-2.56645391643843,0.931661973805637,
1.80598403391229E-16));
#29342=CARTESIAN_POINT('Ctrl Pts',(-2.56264940755798,0.945931896412831,
-2.32436284838826E-16));
#29343=CARTESIAN_POINT('Ctrl Pts',(-2.55872953347648,0.960165880107832,
-2.22044604925031E-16));
#29344=CARTESIAN_POINT('Ctrl Pts',(-2.53414545266093,1.04943645314397,-1.56871618880494E-16));
#29345=CARTESIAN_POINT('Ctrl Pts',(-2.50500995111573,1.13736326277131,-2.05141327217914E-17));
#29346=CARTESIAN_POINT('Ctrl Pts',(-2.4716122792232,1.22366382845986,-2.77555756156289E-17));
#29347=CARTESIAN_POINT('Ctrl Pts',(-2.4375744436594,1.31161859588862,-3.51358218572908E-17));
#29348=CARTESIAN_POINT('Ctrl Pts',(-2.39910931031647,1.39788496430102,-3.16197773120891E-16));
#29349=CARTESIAN_POINT('Ctrl Pts',(-2.35646765233004,1.48216671345376,-3.33066907387547E-16));
#29350=CARTESIAN_POINT('Ctrl Pts',(-2.31346972634883,1.56715263057712,-3.50076982061372E-16));
#29351=CARTESIAN_POINT('Ctrl Pts',(-2.26622490268864,1.65012150115931,-2.40346217807297E-16));
#29352=CARTESIAN_POINT('Ctrl Pts',(-2.21493810777665,1.7307598326539,-2.77555756156289E-16));
#29353=CARTESIAN_POINT('Ctrl Pts',(-2.18420890619665,1.77907541852398,-2.99850372277004E-16));
#29354=CARTESIAN_POINT('Ctrl Pts',(-2.15202766717645,1.82655410022214,-8.23577960215966E-17));
#29355=CARTESIAN_POINT('Ctrl Pts',(-2.11843029730051,1.87312475572319,-1.11022302462516E-16));
#29356=CARTESIAN_POINT('Ctrl Pts',(-2.10910817041026,1.88604652791983,-1.18975727604888E-16));
#29357=CARTESIAN_POINT('Ctrl Pts',(-2.09967596196574,1.89889961347673,3.5091792826265E-16));
#29358=CARTESIAN_POINT('Ctrl Pts',(-2.09014599464406,1.91166724455946,3.33066907387547E-16));
#29359=CARTESIAN_POINT('Ctrl Pts',(-2.03133578634427,1.99045734090759,2.22906796592623E-16));
#29360=CARTESIAN_POINT('Ctrl Pts',(-1.96871406102828,2.0661248657246,1.99254278682365E-16));
#29361=CARTESIAN_POINT('Ctrl Pts',(-1.902552599463,2.13836101844373,1.66533453693773E-16));
#29362=CARTESIAN_POINT('Ctrl Pts',(-1.8362287723598,2.21077444448052,1.33732329173934E-16));
#29363=CARTESIAN_POINT('Ctrl Pts',(-1.76634741320835,2.27974053651805,-4.02039597886661E-17));
#29364=CARTESIAN_POINT('Ctrl Pts',(-1.69313231821204,2.34493242732506,-5.55111512312578E-17));
#29365=CARTESIAN_POINT('Ctrl Pts',(-1.62133085597193,2.40886559693137,-7.05227923200634E-17));
#29366=CARTESIAN_POINT('Ctrl Pts',(-1.54632261932841,2.46916967164754,2.95537804665533E-16));
#29367=CARTESIAN_POINT('Ctrl Pts',(-1.46827783385673,2.52550895680454,3.33066907387547E-16));
#29368=CARTESIAN_POINT('Ctrl Pts',(-1.41015813731654,2.56746463823574,3.6101470746729E-16));
#29369=CARTESIAN_POINT('Ctrl Pts',(-1.35035358675696,2.60722107009064,1.43731543267252E-17));
#29370=CARTESIAN_POINT('Ctrl Pts',(-1.28892185405322,2.64462557919718,0.));
#29371=CARTESIAN_POINT('Origin',(0.,0.,0.));
#29372=CARTESIAN_POINT('Origin',(-1.44337567297407,-2.5,-6.));
#29373=CARTESIAN_POINT('',(-1.44337567297407,-2.5,-6.));
#29374=CARTESIAN_POINT('',(1.44337567297406,-2.5,-6.));
#29375=CARTESIAN_POINT('',(-0.721687836487033,-2.5,-6.));
#29376=CARTESIAN_POINT('',(-1.44337567297407,-2.5,-3.));
#29377=CARTESIAN_POINT('',(-1.44337567297407,-2.5,-6.));
#29378=CARTESIAN_POINT('',(1.44337567297406,-2.5,-3.));
#29379=CARTESIAN_POINT('',(-1.44337567297407,-2.5,-3.));
#29380=CARTESIAN_POINT('',(1.44337567297406,-2.5,-6.));
#29381=CARTESIAN_POINT('Origin',(-2.88675134594813,3.53525079574969E-16,
-6.));
#29382=CARTESIAN_POINT('',(-2.88675134594813,3.53525079574969E-16,-6.));
#29383=CARTESIAN_POINT('',(-2.52590742770461,-0.625,-6.));
#29384=CARTESIAN_POINT('',(-2.88675134594813,5.55111512312578E-16,-3.));
#29385=CARTESIAN_POINT('',(-2.88675134594813,3.53525079574969E-16,-6.));
#29386=CARTESIAN_POINT('',(-2.88675134594813,3.53525079574969E-16,-3.));
#29387=CARTESIAN_POINT('Origin',(-1.44337567297406,2.5,-6.));
#29388=CARTESIAN_POINT('',(-1.44337567297406,2.5,-6.));
#29389=CARTESIAN_POINT('',(-1.80421959121758,1.875,-6.));
#29390=CARTESIAN_POINT('',(-1.44337567297406,2.5,-3.));
#29391=CARTESIAN_POINT('',(-1.44337567297406,2.5,-6.));
#29392=CARTESIAN_POINT('',(-1.44337567297406,2.5,-3.));
#29393=CARTESIAN_POINT('Origin',(1.44337567297406,2.5,-6.));
#29394=CARTESIAN_POINT('',(1.44337567297406,2.5,-6.));
#29395=CARTESIAN_POINT('',(0.721687836487033,2.5,-6.));
#29396=CARTESIAN_POINT('',(1.44337567297406,2.5,-3.));
#29397=CARTESIAN_POINT('',(1.44337567297406,2.5,-6.));
#29398=CARTESIAN_POINT('',(1.44337567297406,2.5,-3.));
#29399=CARTESIAN_POINT('Origin',(2.88675134594813,0.,-6.));
#29400=CARTESIAN_POINT('',(2.88675134594813,0.,-6.));
#29401=CARTESIAN_POINT('',(2.52590742770461,0.625,-6.));
#29402=CARTESIAN_POINT('',(2.88675134594813,0.,-3.));
#29403=CARTESIAN_POINT('',(2.88675134594813,0.,-6.));
#29404=CARTESIAN_POINT('',(2.88675134594813,0.,-3.));
#29405=CARTESIAN_POINT('Origin',(1.44337567297406,-2.5,-6.));
#29406=CARTESIAN_POINT('',(1.80421959121758,-1.875,-6.));
#29407=CARTESIAN_POINT('',(1.44337567297406,-2.5,-3.));
#29408=CARTESIAN_POINT('Origin',(0.,0.,-3.));
#29409=CARTESIAN_POINT('Origin',(0.,0.,0.));
#29410=CARTESIAN_POINT('',(-5.,-6.12323399573677E-16,0.));
#29411=CARTESIAN_POINT('Origin',(0.,0.,0.));
#29412=CARTESIAN_POINT('Origin',(0.,0.,-6.));
#29413=CARTESIAN_POINT('',(-5.,-6.12323399573677E-16,-6.));
#29414=CARTESIAN_POINT('',(-5.,-6.12323399573677E-16,-6.));
#29415=CARTESIAN_POINT('Origin',(0.,0.,-6.));
#29416=CARTESIAN_POINT('Origin',(0.,0.,-6.));
#29417=CARTESIAN_POINT('Origin',(0.,0.,20.));
#29418=CARTESIAN_POINT('',(0.,0.,0.));
#29419=CARTESIAN_POINT('Origin',(0.,0.,0.));
#29420=CARTESIAN_POINT('',(-2.94437861999191,0.00228824954296311,0.322176117089596));
#29421=CARTESIAN_POINT('',(-2.94436911647834,0.00312614869137163,0.177823882910396));
#29422=CARTESIAN_POINT('',(-2.942,-3.60291088309151E-16,0.));
#29423=CARTESIAN_POINT('',(1.28892185405323,2.64462557919717,0.));
#29424=CARTESIAN_POINT('Ctrl Pts',(-2.94437861999191,0.00228824954296311,
0.322176117089596));
#29425=CARTESIAN_POINT('Ctrl Pts',(-2.94551635113874,0.142778583613822,
0.314557432409286));
#29426=CARTESIAN_POINT('Ctrl Pts',(-2.93631267309395,0.283111895578672,
0.306938747728977));
#29427=CARTESIAN_POINT('Ctrl Pts',(-2.91624915612822,0.42186500989966,0.299320063048668));
#29428=CARTESIAN_POINT('Ctrl Pts',(-2.77830971889191,1.37581174500659,0.246940558544163));
#29429=CARTESIAN_POINT('Ctrl Pts',(-2.1270526803082,2.25506646395135,0.194561054039658));
#29430=CARTESIAN_POINT('Ctrl Pts',(-1.25475282359973,2.66583045735473,0.142181549535154));
#29431=CARTESIAN_POINT('Ctrl Pts',(-0.46548135530728,3.03749657388775,0.0947876996901026));
#29432=CARTESIAN_POINT('Ctrl Pts',(0.504756374147381,3.02561249996607,0.0473938498450515));
#29433=CARTESIAN_POINT('Ctrl Pts',(1.29197400994443,2.64783394680711,3.05745012640912E-16));
#29434=CARTESIAN_POINT('',(-1.28892185405326,2.64462557919716,0.));
#29435=CARTESIAN_POINT('Origin',(0.,0.,0.));
#29436=CARTESIAN_POINT('Ctrl Pts',(-1.28892185405326,2.64462557919716,1.87350135405495E-15));
#29437=CARTESIAN_POINT('Ctrl Pts',(-2.16038499609478,2.21989706654312,0.0524451052237091));
#29438=CARTESIAN_POINT('Ctrl Pts',(-2.79846764402885,1.33473338532309,0.104890210447416));
#29439=CARTESIAN_POINT('Ctrl Pts',(-2.92193100282573,0.379041548713593,
0.157335315671123));
#29440=CARTESIAN_POINT('Ctrl Pts',(-2.93800868581449,0.25458915624929,0.164164838084214));
#29441=CARTESIAN_POINT('Ctrl Pts',(-2.94535953294187,0.128940758021734,
0.170994360497305));
#29442=CARTESIAN_POINT('Ctrl Pts',(-2.94436911647834,0.00312614869137163,
0.177823882910396));
#29443=CARTESIAN_POINT('Origin',(0.,0.,0.));
#29444=CARTESIAN_POINT('',(-2.93740032720055,-0.000139020310086779,1.32217611708959));
#29445=CARTESIAN_POINT('',(-2.93737720095951,0.000230872487724698,1.1778238829104));
#29446=CARTESIAN_POINT('',(-2.942,-3.60291088309151E-16,0.));
#29447=CARTESIAN_POINT('Ctrl Pts',(-2.93740032720055,-0.000139020310086779,
1.32217611708959));
#29448=CARTESIAN_POINT('Ctrl Pts',(-2.93718361365059,0.494770241727901,
1.29550112610298));
#29449=CARTESIAN_POINT('Ctrl Pts',(-2.81848923912434,0.989776479202536,
1.26882613511636));
#29450=CARTESIAN_POINT('Ctrl Pts',(-2.58191143461274,1.4199490257311,1.24215114412975));
#29451=CARTESIAN_POINT('Ctrl Pts',(-2.11736289237333,2.26464377557798,1.18977163962524));
#29452=CARTESIAN_POINT('Ctrl Pts',(-1.19827972440715,2.85935294685526,1.13739213512074));
#29453=CARTESIAN_POINT('Ctrl Pts',(-0.2374000875181,2.93702585155106,1.08501263061624));
#29454=CARTESIAN_POINT('Ctrl Pts',(0.723479549370952,3.01469875624685,1.03263312611173));
#29455=CARTESIAN_POINT('Ctrl Pts',(1.72615565518287,2.57533539436116,0.980253621607226));
#29456=CARTESIAN_POINT('Ctrl Pts',(2.32033868002489,1.8162041612206,0.927874117102722));
#29457=CARTESIAN_POINT('Ctrl Pts',(2.9145217048669,1.05707292808004,0.875494612598217));
#29458=CARTESIAN_POINT('Ctrl Pts',(3.100211648739,-0.0218261763153739,0.823115108093712));
#29459=CARTESIAN_POINT('Ctrl Pts',(2.79403320730894,-0.935902477435646,
0.770735603589208));
#29460=CARTESIAN_POINT('Ctrl Pts',(2.48785476587888,-1.84997877855592,0.718356099084703));
#29461=CARTESIAN_POINT('Ctrl Pts',(1.68980793914667,-2.59923227640105,0.665976594580199));
#29462=CARTESIAN_POINT('Ctrl Pts',(0.75825229618776,-2.84733793424016,0.613597090075694));
#29463=CARTESIAN_POINT('Ctrl Pts',(-0.173303346771145,-3.09544359207927,
0.56121758557119));
#29464=CARTESIAN_POINT('Ctrl Pts',(-1.23836780595674,-2.84240140991237,
0.508838081066685));
#29465=CARTESIAN_POINT('Ctrl Pts',(-1.95858911760509,-2.20156094319437,
0.456458576562181));
#29466=CARTESIAN_POINT('Ctrl Pts',(-2.57405306040479,-1.65393177147606,
0.411697756737986));
#29467=CARTESIAN_POINT('Ctrl Pts',(-2.93769429310237,-0.823111776086056,
0.366936936913791));
#29468=CARTESIAN_POINT('Ctrl Pts',(-2.94437861999191,0.00228824954296311,
0.322176117089596));
#29469=CARTESIAN_POINT('Ctrl Pts',(-2.94436911647834,0.00312614869137163,
0.177823882910396));
#29470=CARTESIAN_POINT('Ctrl Pts',(-2.93775395051561,-0.837211781775621,
0.223439465721013));
#29471=CARTESIAN_POINT('Ctrl Pts',(-2.55902339432207,-1.68496462111194,
0.26905504853163));
#29472=CARTESIAN_POINT('Ctrl Pts',(-1.92306539600717,-2.23328718212897,
0.314670631342247));
#29473=CARTESIAN_POINT('Ctrl Pts',(-1.19189236073203,-2.86370408436305,
0.367115736565955));
#29474=CARTESIAN_POINT('Ctrl Pts',(-0.120702220522052,-3.09831789683223,
0.419560841789662));
#29475=CARTESIAN_POINT('Ctrl Pts',(0.807638005699694,-2.8335361097114,0.47200594701337));
#29476=CARTESIAN_POINT('Ctrl Pts',(1.73597823192144,-2.56875432259058,0.524451052237078));
#29477=CARTESIAN_POINT('Ctrl Pts',(2.52146854415495,-1.80457693587975,0.576896157460787));
#29478=CARTESIAN_POINT('Ctrl Pts',(2.81091642121069,-0.883954119006901,
0.629341262684494));
#29479=CARTESIAN_POINT('Ctrl Pts',(3.10036429826643,0.0366686978659464,
0.681786367908202));
#29480=CARTESIAN_POINT('Ctrl Pts',(2.89376974014439,1.11373694490081,0.734231473131909));
#29481=CARTESIAN_POINT('Ctrl Pts',(2.28393241469019,1.86192138048068,0.786676578355617));
#29482=CARTESIAN_POINT('Ctrl Pts',(1.674095089236,2.61010581606054,0.839121683579324));
#29483=CARTESIAN_POINT('Ctrl Pts',(0.661014996449636,3.02940644018541,0.891566788803033));
#29484=CARTESIAN_POINT('Ctrl Pts',(-0.299207810136722,2.93136603044105,
0.944011894026741));
#29485=CARTESIAN_POINT('Ctrl Pts',(-1.25943061672308,2.83332562069669,0.996456999250449));
#29486=CARTESIAN_POINT('Ctrl Pts',(-2.16679613710945,2.21794417708309,1.04890210447416));
#29487=CARTESIAN_POINT('Ctrl Pts',(-2.61293993368518,1.36206873790977,1.10134720969786));
#29488=CARTESIAN_POINT('Ctrl Pts',(-2.82979902340055,0.946049575313678,
1.12683943410204));
#29489=CARTESIAN_POINT('Ctrl Pts',(-2.93768601866802,0.47320929383844,1.15233165850622));
#29490=CARTESIAN_POINT('Ctrl Pts',(-2.93737720095951,0.000230872487724698,
1.1778238829104));
#29491=CARTESIAN_POINT('Origin',(0.,0.,0.));
#29492=CARTESIAN_POINT('',(-2.94487182720719,-0.00190539986535287,2.32217611708959));
#29493=CARTESIAN_POINT('',(-2.94409804542743,-0.00221960462873976,2.1778238829104));
#29494=CARTESIAN_POINT('',(-2.942,-3.60291088309151E-16,0.));
#29495=CARTESIAN_POINT('Ctrl Pts',(-2.94487182720719,-0.00190539986535287,
2.32217611708959));
#29496=CARTESIAN_POINT('Ctrl Pts',(-2.93849254859689,0.841069663508672,
2.27644481979667));
#29497=CARTESIAN_POINT('Ctrl Pts',(-2.55692453936773,1.68909389771769,2.23071352250375));
#29498=CARTESIAN_POINT('Ctrl Pts',(-1.91797659724234,2.23693579382214,2.18498222521083));
#29499=CARTESIAN_POINT('Ctrl Pts',(-1.18614132044426,2.86442044357863,2.13260272070633));
#29500=CARTESIAN_POINT('Ctrl Pts',(-0.116653199765081,3.09810042098425,
2.08022321620182));
#29501=CARTESIAN_POINT('Ctrl Pts',(0.810201861614963,2.83303510458914,2.02784371169732));
#29502=CARTESIAN_POINT('Ctrl Pts',(1.73705692299501,2.56796978819403,1.97546420719281));
#29503=CARTESIAN_POINT('Ctrl Pts',(2.52127892507592,1.80415917799819,1.92308470268831));
#29504=CARTESIAN_POINT('Ctrl Pts',(2.81068910755427,0.88461468761641,1.8707051981838));
#29505=CARTESIAN_POINT('Ctrl Pts',(3.10009929003262,-0.0349298027653776,
1.8183256936793));
#29506=CARTESIAN_POINT('Ctrl Pts',(2.89469765290841,-1.11020817333311,1.76594618917479));
#29507=CARTESIAN_POINT('Ctrl Pts',(2.28672630753671,-1.85833254788295,1.71356668467029));
#29508=CARTESIAN_POINT('Ctrl Pts',(1.67875496216501,-2.60645692243279,1.66118718016578));
#29509=CARTESIAN_POINT('Ctrl Pts',(0.668213908545816,-3.02742730096473,
1.60880767566128));
#29510=CARTESIAN_POINT('Ctrl Pts',(-0.291083395731117,-2.93219727380604,
1.55642817115678));
#29511=CARTESIAN_POINT('Ctrl Pts',(-1.25038070000804,-2.83696724664735,
1.50404866665227));
#29512=CARTESIAN_POINT('Ctrl Pts',(-2.15843425494271,-2.22553681379804,
1.45166916214777));
#29513=CARTESIAN_POINT('Ctrl Pts',(-2.60745407415374,-1.37248143316515,
1.39928965764326));
#29514=CARTESIAN_POINT('Ctrl Pts',(-2.82780430697652,-0.953856366540085,
1.37358514412537));
#29515=CARTESIAN_POINT('Ctrl Pts',(-2.93760915637607,-0.477042717206063,
1.34788063060748));
#29516=CARTESIAN_POINT('Ctrl Pts',(-2.93740032720055,-0.000139020310086779,
1.32217611708959));
#29517=CARTESIAN_POINT('Ctrl Pts',(-2.93737720095951,0.000230872487724698,
1.1778238829104));
#29518=CARTESIAN_POINT('Ctrl Pts',(-2.9370506885783,-0.499848321024544,
1.20477676372993));
#29519=CARTESIAN_POINT('Ctrl Pts',(-2.81577431600542,-1.00008193824477,
1.23172964454946));
#29520=CARTESIAN_POINT('Ctrl Pts',(-2.57446559490686,-1.43347457044749,
1.25868252536899));
#29521=CARTESIAN_POINT('Ctrl Pts',(-2.10492538678771,-2.27677300489839,
1.31112763059269));
#29522=CARTESIAN_POINT('Ctrl Pts',(-1.1809228977843,-2.86700043906715,1.3635727358164));
#29523=CARTESIAN_POINT('Ctrl Pts',(-0.218377608724914,-2.93852741234213,
1.41601784104011));
#29524=CARTESIAN_POINT('Ctrl Pts',(0.744167680334467,-3.01005438561711,
1.46846294626382));
#29525=CARTESIAN_POINT('Ctrl Pts',(1.74525576944982,-2.56288089799832,1.52090805148753));
#29526=CARTESIAN_POINT('Ctrl Pts',(2.33429173832943,-1.79826479808332,1.57335315671123));
#29527=CARTESIAN_POINT('Ctrl Pts',(2.92332770720905,-1.03364869816832,1.62579826193494));
#29528=CARTESIAN_POINT('Ctrl Pts',(3.10031155585293,0.0484100140428809,
1.67824336715865));
#29529=CARTESIAN_POINT('Ctrl Pts',(2.78557670999694,0.960852278151669,1.73068847238236));
#29530=CARTESIAN_POINT('Ctrl Pts',(2.47084186414094,1.87329454226046,1.78313357760607));
#29531=CARTESIAN_POINT('Ctrl Pts',(1.66438832378506,2.61612035826684,1.83557868282977));
#29532=CARTESIAN_POINT('Ctrl Pts',(0.729213057861966,2.85498007465664,1.88802378805348));
#29533=CARTESIAN_POINT('Ctrl Pts',(-0.205962208061124,3.09383979104644,
1.94046889327719));
#29534=CARTESIAN_POINT('Ctrl Pts',(-1.26985919955142,2.82873340781965,1.9929139985009));
#29535=CARTESIAN_POINT('Ctrl Pts',(-1.98360551176881,2.17898571169394,2.0453591037246));
#29536=CARTESIAN_POINT('Ctrl Pts',(-2.58452748049057,1.63194587688865,2.08951403011987));
#29537=CARTESIAN_POINT('Ctrl Pts',(-2.93724853244873,0.81225677381718,2.13366895651513));
#29538=CARTESIAN_POINT('Ctrl Pts',(-2.94409804542743,-0.00221960462873976,
2.1778238829104));
#29539=CARTESIAN_POINT('Origin',(0.,0.,0.));
#29540=CARTESIAN_POINT('',(-2.94188729812012,0.00254759896953657,3.32217611708959));
#29541=CARTESIAN_POINT('',(-2.94300132914192,0.00247067809074119,3.17782388291039));
#29542=CARTESIAN_POINT('',(-2.942,-3.60291088309151E-16,0.));
#29543=CARTESIAN_POINT('Ctrl Pts',(-2.94188729812012,0.00254759896953657,
3.32217611708959));
#29544=CARTESIAN_POINT('Ctrl Pts',(-2.94391723822425,0.231870355671395,
3.30976801799487));
#29545=CARTESIAN_POINT('Ctrl Pts',(-2.91930872547992,0.460762551320829,
3.29735991890015));
#29546=CARTESIAN_POINT('Ctrl Pts',(-2.86638309031571,0.682908266801983,
3.28495181980542));
#29547=CARTESIAN_POINT('Ctrl Pts',(-2.64296300603654,1.62067338423639,3.23257231530092));
#29548=CARTESIAN_POINT('Ctrl Pts',(-1.91492649555138,2.438214961245,3.18019281079642));
#29549=CARTESIAN_POINT('Ctrl Pts',(-1.00922037183541,2.76839122410029,3.12781330629191));
#29550=CARTESIAN_POINT('Ctrl Pts',(-0.103514248119433,3.09856748695557,
3.07543380178741));
#29551=CARTESIAN_POINT('Ctrl Pts',(0.979861488827348,2.94137843565753,3.0230542972829));
#29552=CARTESIAN_POINT('Ctrl Pts',(1.75438420282982,2.3674145763557,2.9706747927784));
#29553=CARTESIAN_POINT('Ctrl Pts',(2.5289069168323,1.79345071705387,2.91829528827389));
#29554=CARTESIAN_POINT('Ctrl Pts',(2.99457660789046,0.802712049748258,2.86591578376939));
#29555=CARTESIAN_POINT('Ctrl Pts',(2.94227021542597,-0.159880282562335,
2.81353627926488));
#29556=CARTESIAN_POINT('Ctrl Pts',(2.88996382296149,-1.12247261487293,2.76115677476038));
#29557=CARTESIAN_POINT('Ctrl Pts',(2.31968134697434,-2.0569186121885,2.70877727025587));
#29558=CARTESIAN_POINT('Ctrl Pts',(1.48752538566269,-2.54357700727495,2.65639776575137));
#29559=CARTESIAN_POINT('Ctrl Pts',(0.655369424351043,-3.0302354023614,2.60401826124687));
#29560=CARTESIAN_POINT('Ctrl Pts',(-0.438660022285117,-3.06910619521874,
2.55163875674236));
#29561=CARTESIAN_POINT('Ctrl Pts',(-1.30325595742871,-2.64273334365957,
2.49925925223786));
#29562=CARTESIAN_POINT('Ctrl Pts',(-2.1678518925723,-2.21636049210041,2.44687974773335));
#29563=CARTESIAN_POINT('Ctrl Pts',(-2.80301431622333,-1.32474399612474,
2.39450024322885));
#29564=CARTESIAN_POINT('Ctrl Pts',(-2.92350431159035,-0.368291087083228,
2.34212073872434));
#29565=CARTESIAN_POINT('Ctrl Pts',(-2.93879736301763,-0.246894422727957,
2.33547253151276));
#29566=CARTESIAN_POINT('Ctrl Pts',(-2.94579921760659,-0.124453265927633,
2.32882432430118));
#29567=CARTESIAN_POINT('Ctrl Pts',(-2.94487182720719,-0.00190539986535287,
2.32217611708959));
#29568=CARTESIAN_POINT('Ctrl Pts',(-2.94409804542743,-0.00221960462873976,
2.1778238829104));
#29569=CARTESIAN_POINT('Ctrl Pts',(-2.94538405566721,-0.155139230593375,
2.18611406173884));
#29570=CARTESIAN_POINT('Ctrl Pts',(-2.93447780370748,-0.307875103637501,
2.19440424056728));
#29571=CARTESIAN_POINT('Ctrl Pts',(-2.91073286453113,-0.458588216909009,
2.20269441939573));
#29572=CARTESIAN_POINT('Ctrl Pts',(-2.76051827213159,-1.41202544036162,
2.25513952461944));
#29573=CARTESIAN_POINT('Ctrl Pts',(-2.09649345438802,-2.28451087824219,
2.30758462984315));
#29574=CARTESIAN_POINT('Ctrl Pts',(-1.21754466145652,-2.68332862013697,
2.36002973506685));
#29575=CARTESIAN_POINT('Ctrl Pts',(-0.338595868525027,-3.08214636203174,
2.41247484029056));
#29576=CARTESIAN_POINT('Ctrl Pts',(0.755276899594388,-3.00729640794073,
2.46491994551426));
#29577=CARTESIAN_POINT('Ctrl Pts',(1.57170784623814,-2.49246924635079,2.51736505073797));
#29578=CARTESIAN_POINT('Ctrl Pts',(2.3881387928819,-1.97764208476085,2.56981015596168));
#29579=CARTESIAN_POINT('Ctrl Pts',(2.92712791805,-1.02283771567197,2.62225526118539));
#29580=CARTESIAN_POINT('Ctrl Pts',(2.94606932856971,-0.0578258660348382,
2.6747003664091));
#29581=CARTESIAN_POINT('Ctrl Pts',(2.96501073908941,0.907185983602299,2.72714547163281));
#29582=CARTESIAN_POINT('Ctrl Pts',(2.46390443496074,1.88240531378769,2.77959057685651));
#29583=CARTESIAN_POINT('Ctrl Pts',(1.66830473495772,2.42887370127543,2.83203568208022));
#29584=CARTESIAN_POINT('Ctrl Pts',(0.872705034954712,2.97534208876317,2.88448078730393));
#29585=CARTESIAN_POINT('Ctrl Pts',(-0.217388060922636,3.09305953355326,
2.93692589252764));
#29586=CARTESIAN_POINT('Ctrl Pts',(-1.11130990317228,2.72903986659667,2.98937099775135));
#29587=CARTESIAN_POINT('Ctrl Pts',(-2.00523174542191,2.36502019964009,3.04181610297505));
#29588=CARTESIAN_POINT('Ctrl Pts',(-2.70298233404385,1.51926342093683,3.09426120819876));
#29589=CARTESIAN_POINT('Ctrl Pts',(-2.89049530439613,0.572455370821353,
3.14670631342247));
#29590=CARTESIAN_POINT('Ctrl Pts',(-2.92758137029262,0.385196933861252,
3.15707883658511));
#29591=CARTESIAN_POINT('Ctrl Pts',(-2.94470877622731,0.1939857347123,3.16745135974775));
#29592=CARTESIAN_POINT('Ctrl Pts',(-2.94300132914192,0.00247067809074119,
3.17782388291039));
#29593=CARTESIAN_POINT('Origin',(0.,0.,0.));
#29594=CARTESIAN_POINT('',(-2.93815144027097,-0.00144838940242836,4.32217611708959));
#29595=CARTESIAN_POINT('',(-2.93758805006728,-0.000810565913221897,4.1778238829104));
#29596=CARTESIAN_POINT('',(-2.942,-3.60291088309151E-16,0.));
#29597=CARTESIAN_POINT('Ctrl Pts',(-2.93815144027097,-0.00144838940242836,
4.32217611708959));
#29598=CARTESIAN_POINT('Ctrl Pts',(-2.93549507201127,0.581944663119171,
4.29071171168856));
#29599=CARTESIAN_POINT('Ctrl Pts',(-2.76704590305946,1.16675179323199,4.25924730628754));
#29600=CARTESIAN_POINT('Ctrl Pts',(-2.44338137442995,1.64693751569171,4.22778290088651));
#29601=CARTESIAN_POINT('Ctrl Pts',(-1.90456974207211,2.44631350554451,4.175403396382));
#29602=CARTESIAN_POINT('Ctrl Pts',(-0.93560961338887,2.95575207374732,4.1230238918775));
#29603=CARTESIAN_POINT('Ctrl Pts',(0.0283581627927666,2.94647442485208,
4.07064438737299));
#29604=CARTESIAN_POINT('Ctrl Pts',(0.992325938974403,2.93719677595684,4.01826488286848));
#29605=CARTESIAN_POINT('Ctrl Pts',(1.95130136265442,2.40920290996356,3.96588537836398));
#29606=CARTESIAN_POINT('Ctrl Pts',(2.4746275187937,1.59960444002515,3.91350587385948));
#29607=CARTESIAN_POINT('Ctrl Pts',(2.99795367493297,0.790005970086747,3.86112636935497));
#29608=CARTESIAN_POINT('Ctrl Pts',(3.0856305635315,-0.301197103796779,3.80874686485047));
#29609=CARTESIAN_POINT('Ctrl Pts',(2.69828422619929,-1.18396704178881,3.75636736034596));
#29610=CARTESIAN_POINT('Ctrl Pts',(2.31093788886708,-2.06673697978085,3.70398785584146));
#29611=CARTESIAN_POINT('Ctrl Pts',(1.44856832560414,-2.7410737818814,3.65160835133695));
#29612=CARTESIAN_POINT('Ctrl Pts',(0.498448668458934,-2.90414611332682,
3.59922884683245));
#29613=CARTESIAN_POINT('Ctrl Pts',(-0.451670988686273,-3.06721844477224,
3.54684934232795));
#29614=CARTESIAN_POINT('Ctrl Pts',(-1.48954073971375,-2.71902630556253,
3.49446983782344));
#29615=CARTESIAN_POINT('Ctrl Pts',(-2.1490737861909,-2.01593590702758,3.44209033331894));
#29616=CARTESIAN_POINT('Ctrl Pts',(-2.65237107835254,-1.47939949597489,
3.40211892790916));
#29617=CARTESIAN_POINT('Ctrl Pts',(-2.93534805643284,-0.736191897535303,
3.36214752249938));
#29618=CARTESIAN_POINT('Ctrl Pts',(-2.94188729812012,0.00254759896953657,
3.32217611708959));
#29619=CARTESIAN_POINT('Ctrl Pts',(-2.94300132914192,0.00247067809074119,
3.17782388291039));
#29620=CARTESIAN_POINT('Ctrl Pts',(-2.93607565575577,-0.774344452547842,
3.21989646497146));
#29621=CARTESIAN_POINT('Ctrl Pts',(-2.61927127105561,-1.55615877069983,
3.26196904703253));
#29622=CARTESIAN_POINT('Ctrl Pts',(-2.06758380697847,-2.0994678941542,3.30404162909359));
#29623=CARTESIAN_POINT('Ctrl Pts',(-1.37988398712591,-2.77672378748653,
3.3564867343173));
#29624=CARTESIAN_POINT('Ctrl Pts',(-0.327208995338195,-3.08337625262348,
3.40893183954101));
#29625=CARTESIAN_POINT('Ctrl Pts',(0.616618861412321,-2.88139713307019,
3.46137694476472));
#29626=CARTESIAN_POINT('Ctrl Pts',(1.56044671816283,-2.67941801351691,3.51382204998842));
#29627=CARTESIAN_POINT('Ctrl Pts',(2.39542743987614,-1.9688073092734,3.56626715521213));
#29628=CARTESIAN_POINT('Ctrl Pts',(2.74572565546219,-1.06941987852551,3.61871226043584));
#29629=CARTESIAN_POINT('Ctrl Pts',(3.09602387104824,-0.170032447777603,
3.67115736565955));
#29630=CARTESIAN_POINT('Ctrl Pts',(2.96163958050702,0.918131709474696,3.72360247088326));
#29631=CARTESIAN_POINT('Ctrl Pts',(2.40306085127007,1.70527616384954,3.77604757610696));
#29632=CARTESIAN_POINT('Ctrl Pts',(1.84448212203313,2.49242061822439,3.82849268133067));
#29633=CARTESIAN_POINT('Ctrl Pts',(0.86170895410048,2.97854536972178,3.88093778655438));
#29634=CARTESIAN_POINT('Ctrl Pts',(-0.10290003671811,2.94483952623603,3.93338289177809));
#29635=CARTESIAN_POINT('Ctrl Pts',(-1.06750902753671,2.91113368275028,3.98582799700179));
#29636=CARTESIAN_POINT('Ctrl Pts',(-2.01395384124124,2.35759724428137,4.0382731022255));
#29637=CARTESIAN_POINT('Ctrl Pts',(-2.51622771244025,1.53338395412712,4.09071820744921));
#29638=CARTESIAN_POINT('Ctrl Pts',(-2.79430199366995,1.07707409733029,4.11975343260294));
#29639=CARTESIAN_POINT('Ctrl Pts',(-2.9362347477918,0.537799876108109,4.14878865775667));
#29640=CARTESIAN_POINT('Ctrl Pts',(-2.93758805006728,-0.000810565913221897,
4.1778238829104));
#29641=CARTESIAN_POINT('Origin',(0.,0.,0.));
#29642=CARTESIAN_POINT('',(-2.94644869531747,-0.000604754645607275,5.3221761170896));
#29643=CARTESIAN_POINT('',(-2.945679792052,-0.00146169071580815,5.1778238829104));
#29644=CARTESIAN_POINT('',(-2.942,-3.60291088309151E-16,0.));
#29645=CARTESIAN_POINT('Ctrl Pts',(-2.94644869531747,-0.000604754645607275,
5.3221761170896));
#29646=CARTESIAN_POINT('Ctrl Pts',(-2.94379550054715,0.929335583914262,
5.27165540538226));
#29647=CARTESIAN_POINT('Ctrl Pts',(-2.46604729438678,1.86162808593007,5.22113469367492));
#29648=CARTESIAN_POINT('Ctrl Pts',(-1.70849336410036,2.40074283220066,5.17061398196758));
#29649=CARTESIAN_POINT('Ctrl Pts',(-0.923066988207087,2.95969305927406,
5.11823447746308));
#29650=CARTESIAN_POINT('Ctrl Pts',(0.163133494924937,3.09600115191732,5.06585497295858));
#29651=CARTESIAN_POINT('Ctrl Pts',(1.06231690977038,2.74845383893534,5.01347546845407));
#29652=CARTESIAN_POINT('Ctrl Pts',(1.96150032461582,2.40090652595338,4.96109596394957));
#29653=CARTESIAN_POINT('Ctrl Pts',(2.67366667117468,1.56950380734618,4.90871645944506));
#29654=CARTESIAN_POINT('Ctrl Pts',(2.87899611438783,0.627612216959094,4.85633695494056));
#29655=CARTESIAN_POINT('Ctrl Pts',(3.08432555760098,-0.314279373428012,
4.80395745043605));
#29656=CARTESIAN_POINT('Ctrl Pts',(2.7828180974684,-1.36665983559502,4.75157794593155));
#29657=CARTESIAN_POINT('Ctrl Pts',(2.10987477706647,-2.05692589721429,4.69919844142705));
#29658=CARTESIAN_POINT('Ctrl Pts',(1.43693145666455,-2.74719195883355,4.64681893692254));
#29659=CARTESIAN_POINT('Ctrl Pts',(0.392552275993288,-3.07534361990509,
4.59443943241804));
#29660=CARTESIAN_POINT('Ctrl Pts',(-0.554252710038128,-2.89401445313919,
4.54205992791353));
#29661=CARTESIAN_POINT('Ctrl Pts',(-1.50105769606954,-2.71268528637328,
4.48968042340903));
#29662=CARTESIAN_POINT('Ctrl Pts',(-2.35028848746111,-2.02187529176995,
4.43730091890452));
#29663=CARTESIAN_POINT('Ctrl Pts',(-2.72057231514067,-1.13181358871689,
4.38492141440002));
#29664=CARTESIAN_POINT('Ctrl Pts',(-2.86842638565151,-0.776412580180032,
4.36400631529654));
#29665=CARTESIAN_POINT('Ctrl Pts',(-2.93991718809614,-0.389242894153138,
4.34309121619307));
#29666=CARTESIAN_POINT('Ctrl Pts',(-2.93815144027097,-0.00144838940242836,
4.32217611708959));
#29667=CARTESIAN_POINT('Ctrl Pts',(-2.93758805006728,-0.000810565913221897,
4.1778238829104));
#29668=CARTESIAN_POINT('Ctrl Pts',(-2.93867916073716,-0.435069497448956,
4.20123376298038));
#29669=CARTESIAN_POINT('Ctrl Pts',(-2.84838634229403,-0.86889693810433,
4.22464364305035));
#29670=CARTESIAN_POINT('Ctrl Pts',(-2.66438363654231,-1.25846258937073,
4.24805352312033));
#29671=CARTESIAN_POINT('Ctrl Pts',(-2.25216276075188,-2.13120570087471,
4.30049862834404));
#29672=CARTESIAN_POINT('Ctrl Pts',(-1.36961808047753,-2.78180178204309,
4.35294373356775));
#29673=CARTESIAN_POINT('Ctrl Pts',(-0.413994103635433,-2.91740931891088,
4.40538883879146));
#29674=CARTESIAN_POINT('Ctrl Pts',(0.541629873206673,-3.05301685577867,
4.45783394401517));
#29675=CARTESIAN_POINT('Ctrl Pts',(1.57033314661653,-2.67363584834587,4.51027904923887));
#29676=CARTESIAN_POINT('Ctrl Pts',(2.20908337968645,-1.9500304800975,4.56272415446258));
#29677=CARTESIAN_POINT('Ctrl Pts',(2.84783361275636,-1.22642511184914,4.61516925968629));
#29678=CARTESIAN_POINT('Ctrl Pts',(3.09663080548633,-0.158595382785209,
4.66761436491));
#29679=CARTESIAN_POINT('Ctrl Pts',(2.84348819889812,0.772815058373636,4.7200594701337));
#29680=CARTESIAN_POINT('Ctrl Pts',(2.5903455923099,1.70422549953248,4.77250457535741));
#29681=CARTESIAN_POINT('Ctrl Pts',(1.83526318640351,2.49921665278624,4.82494968058112));
#29682=CARTESIAN_POINT('Ctrl Pts',(0.918113109485756,2.79995295852677,4.87739478580482));
#29683=CARTESIAN_POINT('Ctrl Pts',(0.000963032567994487,3.1006892642673,
4.92983989102853));
#29684=CARTESIAN_POINT('Ctrl Pts',(-1.07825471536113,2.90717072249458,4.98228499625224));
#29685=CARTESIAN_POINT('Ctrl Pts',(-1.83377059439506,2.30650247319915,5.03473010147595));
#29686=CARTESIAN_POINT('Ctrl Pts',(-2.5208993779335,1.76020496324304,5.08242802862077));
#29687=CARTESIAN_POINT('Ctrl Pts',(-2.94027519175655,0.877129838501974,
5.13012595576559));
#29688=CARTESIAN_POINT('Ctrl Pts',(-2.945679792052,-0.00146169071580815,
5.1778238829104));
#29689=CARTESIAN_POINT('Origin',(0.,0.,0.));
#29690=CARTESIAN_POINT('',(-2.93949980478958,0.00219056232359141,6.3221761170896));
#29691=CARTESIAN_POINT('',(-2.94109090649655,0.00253660757586993,6.1778238829104));
#29692=CARTESIAN_POINT('',(-2.942,-3.60291088309151E-16,0.));
#29693=CARTESIAN_POINT('Ctrl Pts',(-2.93949980478958,0.00219056232359141,
6.3221761170896));
#29694=CARTESIAN_POINT('Ctrl Pts',(-2.94176361798241,0.320687415620876,
6.30497860358046));
#29695=CARTESIAN_POINT('Ctrl Pts',(-2.89395610782771,0.638523376129415,
6.28778109007132));
#29696=CARTESIAN_POINT('Ctrl Pts',(-2.79314214575126,0.938548174128603,
6.27058357656218));
#29697=CARTESIAN_POINT('Ctrl Pts',(-2.48608697885785,1.85235180335153,6.21820407205768));
#29698=CARTESIAN_POINT('Ctrl Pts',(-1.68730919078036,2.60092740470414,6.16582456755317));
#29699=CARTESIAN_POINT('Ctrl Pts',(-0.75552410366601,2.84810446618733,6.11344506304867));
#29700=CARTESIAN_POINT('Ctrl Pts',(0.176260983448343,3.09528152767051,6.06106555854416));
#29701=CARTESIAN_POINT('Ctrl Pts',(1.24105336959955,2.84106004928427,6.00868605403966));
#29702=CARTESIAN_POINT('Ctrl Pts',(1.96067583262663,2.19960587399116,5.95630654953515));
#29703=CARTESIAN_POINT('Ctrl Pts',(2.68029829565369,1.55815169869806,5.90392704503064));
#29704=CARTESIAN_POINT('Ctrl Pts',(3.05475083555665,0.52946482649812,5.85154754052614));
#29705=CARTESIAN_POINT('Ctrl Pts',(2.91587421520356,-0.424491793382225,
5.79916803602164));
#29706=CARTESIAN_POINT('Ctrl Pts',(2.77699759485047,-1.37844841326258,5.74678853151713));
#29707=CARTESIAN_POINT('Ctrl Pts',(2.12479181424134,-2.25767478082334,5.69440902701263));
#29708=CARTESIAN_POINT('Ctrl Pts',(1.25214960298458,-2.66732770639159,5.64202952250812));
#29709=CARTESIAN_POINT('Ctrl Pts',(0.379507391727844,-3.07698063195983,
5.58965001800362));
#29710=CARTESIAN_POINT('Ctrl Pts',(-0.713571250176501,-3.01706011553558,
5.53727051349912));
#29711=CARTESIAN_POINT('Ctrl Pts',(-1.53620630199898,-2.5144752771182,5.48489100899462));
#29712=CARTESIAN_POINT('Ctrl Pts',(-2.35884135382146,-2.01189043870081,
5.43251150449011));
#29713=CARTESIAN_POINT('Ctrl Pts',(-2.91103281556208,-1.0666412782903,5.3801319999856));
#29714=CARTESIAN_POINT('Ctrl Pts',(-2.94480241210512,-0.103220517333276,
5.3277524954811));
#29715=CARTESIAN_POINT('Ctrl Pts',(-2.94600079462919,-0.069031580495304,
5.32589370268393));
#29716=CARTESIAN_POINT('Ctrl Pts',(-2.94654631348559,-0.0348197596345374,
5.32403490988676));
#29717=CARTESIAN_POINT('Ctrl Pts',(-2.94644869531747,-0.000604754645607275,
5.3221761170896));
#29718=CARTESIAN_POINT('Ctrl Pts',(-2.945679792052,-0.00146169071580815,
5.1778238829104));
#29719=CARTESIAN_POINT('Ctrl Pts',(-2.94621768964176,-0.0889042840834332,
5.18257106098929));
#29720=CARTESIAN_POINT('Ctrl Pts',(-2.94265503660913,-0.176302465642187,
5.18731823906819));
#29721=CARTESIAN_POINT('Ctrl Pts',(-2.93484768462379,-0.263319805187537,
5.19206541714708));
#29722=CARTESIAN_POINT('Ctrl Pts',(-2.84859488567985,-1.22465587746066,
5.24451052237078));
#29723=CARTESIAN_POINT('Ctrl Pts',(-2.24427527765324,-2.13951006518879,
5.29695562759449));
#29724=CARTESIAN_POINT('Ctrl Pts',(-1.39390074925371,-2.59609494298297,
5.34940073281819));
#29725=CARTESIAN_POINT('Ctrl Pts',(-0.543526220854162,-3.05267982077716,
5.4018458380419));
#29726=CARTESIAN_POINT('Ctrl Pts',(0.552903227918311,-3.05099538863739,
5.45429094326562));
#29727=CARTESIAN_POINT('Ctrl Pts',(1.40187085321134,-2.59179983074767,5.50673604848932));
#29728=CARTESIAN_POINT('Ctrl Pts',(2.25083847850436,-2.13260427285796,5.55918115371303));
#29729=CARTESIAN_POINT('Ctrl Pts',(2.85234428031795,-1.21589758921833,5.61162625893673));
#29730=CARTESIAN_POINT('Ctrl Pts',(2.93564289965894,-0.254301037021637,
5.66407136416044));
#29731=CARTESIAN_POINT('Ctrl Pts',(3.01894151899992,0.707295515175046,5.71651646938415));
#29732=CARTESIAN_POINT('Ctrl Pts',(2.5840329558683,1.71378193592877,5.76896157460786));
#29733=CARTESIAN_POINT('Ctrl Pts',(1.82667504784324,2.31212597436553,5.82140667983157));
#29734=CARTESIAN_POINT('Ctrl Pts',(1.06931713981816,2.9104700128023,5.87385178505528));
#29735=CARTESIAN_POINT('Ctrl Pts',(-0.010490113100349,3.1006716689221,5.92629689027898));
#29736=CARTESIAN_POINT('Ctrl Pts',(-0.92671182736886,2.79711877487579,5.97874199550269));
#29737=CARTESIAN_POINT('Ctrl Pts',(-1.84293354163737,2.49356588082949,6.0311871007264));
#29738=CARTESIAN_POINT('Ctrl Pts',(-2.59556971725588,1.69625843661705,6.08363220595011));
#29739=CARTESIAN_POINT('Ctrl Pts',(-2.84584930505901,0.764074593638618,
6.13607731117382));
#29740=CARTESIAN_POINT('Ctrl Pts',(-2.91225724864025,0.516733559576513,
6.14999283508601));
#29741=CARTESIAN_POINT('Ctrl Pts',(-2.94329794130529,0.259896865352817,
6.16390835899821));
#29742=CARTESIAN_POINT('Ctrl Pts',(-2.94109090649655,0.00253660757586993,
6.1778238829104));
#29743=CARTESIAN_POINT('Origin',(0.,0.,0.));
#29744=CARTESIAN_POINT('',(-2.93998607517527,-0.0023358300504342,7.3221761170896));
#29745=CARTESIAN_POINT('',(-2.93846014819028,-0.00170708260597003,7.1778238829104));
#29746=CARTESIAN_POINT('',(-2.942,-3.60291088309151E-16,0.));
#29747=CARTESIAN_POINT('Ctrl Pts',(-2.93998607517527,-0.0023358300504342,
7.3221761170896));
#29748=CARTESIAN_POINT('Ctrl Pts',(-2.93483565594967,0.668801419715884,
7.28592229727415));
#29749=CARTESIAN_POINT('Ctrl Pts',(-2.70624449366069,1.34311250814063,7.2496684774587));
#29750=CARTESIAN_POINT('Ctrl Pts',(-2.28495024526271,1.86051554631288,7.21341465764326));
#29751=CARTESIAN_POINT('Ctrl Pts',(-1.67626448210673,2.60805925085354,7.16103515313876));
#29752=CARTESIAN_POINT('Ctrl Pts',(-0.665321452888303,3.02806588999372,
7.10865564863425));
#29753=CARTESIAN_POINT('Ctrl Pts',(0.293884302746592,2.93191878092119,7.05627614412975));
#29754=CARTESIAN_POINT('Ctrl Pts',(1.25309005838148,2.83577167184866,7.00389663962524));
#29755=CARTESIAN_POINT('Ctrl Pts',(2.16055854043283,2.22347081456344,6.95151713512074));
#29756=CARTESIAN_POINT('Ctrl Pts',(2.60876358347624,1.3699884259484,6.89913763061623));
#29757=CARTESIAN_POINT('Ctrl Pts',(3.05696862651966,0.516506037333356,6.84675812611173));
#29758=CARTESIAN_POINT('Ctrl Pts',(3.04591023055511,-0.578157882611513,
6.79437862160723));
#29759=CARTESIAN_POINT('Ctrl Pts',(2.58055450279311,-1.42241139605186,6.74199911710272));
#29760=CARTESIAN_POINT('Ctrl Pts',(2.11519877503111,-2.26666490949219,6.68961961259822));
#29761=CARTESIAN_POINT('Ctrl Pts',(1.19554571547167,-2.86050801642801,6.63724010809371));
#29762=CARTESIAN_POINT('Ctrl Pts',(0.234593342362696,-2.93725751088208,
6.5848606035892));
#29763=CARTESIAN_POINT('Ctrl Pts',(-0.726359030746288,-3.01400700533615,
6.5324810990847));
#29764=CARTESIAN_POINT('Ctrl Pts',(-1.72861071740481,-2.57366288730847,
6.4801015945802));
#29765=CARTESIAN_POINT('Ctrl Pts',(-2.32207028787941,-1.813974999748,6.4277220900757));
#29766=CARTESIAN_POINT('Ctrl Pts',(-2.72068210106971,-1.30371182195979,
6.39254009908033));
#29767=CARTESIAN_POINT('Ctrl Pts',(-2.93486858555413,-0.649377666932483,
6.35735810808496));
#29768=CARTESIAN_POINT('Ctrl Pts',(-2.93949980478958,0.00219056232359141,
6.3221761170896));
#29769=CARTESIAN_POINT('Ctrl Pts',(-2.94109090649655,0.00253660757586993,
6.1778238829104));
#29770=CARTESIAN_POINT('Ctrl Pts',(-2.9349800243151,-0.710047628629508,
6.21635346422191));
#29771=CARTESIAN_POINT('Ctrl Pts',(-2.67397994955092,-1.42664569379386,
6.25488304553342));
#29772=CARTESIAN_POINT('Ctrl Pts',(-2.20308134670334,-1.95680883878727,
6.29341262684494));
#29773=CARTESIAN_POINT('Ctrl Pts',(-1.5621108005568,-2.67844818649031,6.34585773206864));
#29774=CARTESIAN_POINT('Ctrl Pts',(-0.532246708275948,-3.05466664015197,
6.39830283729235));
#29775=CARTESIAN_POINT('Ctrl Pts',(0.42295609402977,-2.91612352177857,6.45074794251606));
#29776=CARTESIAN_POINT('Ctrl Pts',(1.3781588963355,-2.77758040340517,6.50319304773977));
#29777=CARTESIAN_POINT('Ctrl Pts',(2.25870040866608,-2.12427571299673,6.55563815296348));
#29778=CARTESIAN_POINT('Ctrl Pts',(2.66823777423309,-1.25027014357196,6.60808325818718));
#29779=CARTESIAN_POINT('Ctrl Pts',(3.07777513980009,-0.376264574147203,
6.66052836341089));
#29780=CARTESIAN_POINT('Ctrl Pts',(3.01630835860352,0.718441874293864,6.7129734686346));
#29781=CARTESIAN_POINT('Ctrl Pts',(2.51150440524776,1.54110800210975,6.76541857385831));
#29782=CARTESIAN_POINT('Ctrl Pts',(2.006700451892,2.36377412992563,6.81786367908202));
#29783=CARTESIAN_POINT('Ctrl Pts',(1.05855932637705,2.91439993711633,6.87030878430572));
#29784=CARTESIAN_POINT('Ctrl Pts',(0.0938513252260113,2.94514179293546,
6.92275388952943));
#29785=CARTESIAN_POINT('Ctrl Pts',(-0.870856675925038,2.9758836487546,6.97519899475314));
#29786=CARTESIAN_POINT('Ctrl Pts',(-1.85213155271217,2.48674155320215,7.02764409997685));
#29787=CARTESIAN_POINT('Ctrl Pts',(-2.40828908863565,1.69788454181399,7.08008920520056));
#29788=CARTESIAN_POINT('Ctrl Pts',(-2.75376700818296,1.2078566962645,7.11266743110384));
#29789=CARTESIAN_POINT('Ctrl Pts',(-2.93520341737875,0.60217681128353,7.14524565700712));
#29790=CARTESIAN_POINT('Ctrl Pts',(-2.93846014819028,-0.00170708260597003,
7.1778238829104));
#29791=CARTESIAN_POINT('Origin',(0.,0.,0.));
#29792=CARTESIAN_POINT('',(-2.94622250669394,0.000937675328142526,8.3221761170896));
#29793=CARTESIAN_POINT('',(-2.94656696235233,-0.000396508504380587,8.1778238829104));
#29794=CARTESIAN_POINT('',(-2.942,-3.60291088309151E-16,0.));
#29795=CARTESIAN_POINT('Ctrl Pts',(-2.94622250669394,0.000937675328142526,
8.3221761170896));
#29796=CARTESIAN_POINT('Ctrl Pts',(-2.94645073222768,0.0548930361868928,
8.31924549547236));
#29797=CARTESIAN_POINT('Ctrl Pts',(-2.94509413407217,0.108836699779164,
8.31631487385511));
#29798=CARTESIAN_POINT('Ctrl Pts',(-2.94211616003438,0.162690705921765,
8.31338425223786));
#29799=CARTESIAN_POINT('Ctrl Pts',(-2.88889031756852,1.12523262560549,8.26100474773336));
#29800=CARTESIAN_POINT('Ctrl Pts',(-2.31771549444688,2.05913344782865,8.20862524322884));
#29801=CARTESIAN_POINT('Ctrl Pts',(-1.48509504480843,2.54499674522788,8.15624573872434));
#29802=CARTESIAN_POINT('Ctrl Pts',(-0.652474595169965,3.03086004262711,
8.10386623421983));
#29803=CARTESIAN_POINT('Ctrl Pts',(0.44159148098532,3.06868581520241,8.05148672971533));
#29804=CARTESIAN_POINT('Ctrl Pts',(1.30577973958019,2.64148726651903,7.99910722521083));
#29805=CARTESIAN_POINT('Ctrl Pts',(2.16996799817506,2.21428871783565,7.94672772070633));
#29806=CARTESIAN_POINT('Ctrl Pts',(2.8042784392095,1.3220658478936,7.89434821620182));
#29807=CARTESIAN_POINT('Ctrl Pts',(2.92385476924452,0.36549831322338,7.84196871169732));
#29808=CARTESIAN_POINT('Ctrl Pts',(3.04343109927954,-0.591069221446826,
7.78958920719281));
#29809=CARTESIAN_POINT('Ctrl Pts',(2.64827331831513,-1.61198142084519,7.73720970268831));
#29810=CARTESIAN_POINT('Ctrl Pts',(1.9158389819387,-2.23876678477201,7.68483019818381));
#29811=CARTESIAN_POINT('Ctrl Pts',(1.18340464556226,-2.86555214869884,7.6324506936793));
#29812=CARTESIAN_POINT('Ctrl Pts',(0.113693753773775,-3.09821067715411,
7.58007118917479));
#29813=CARTESIAN_POINT('Ctrl Pts',(-0.812907669552306,-2.83226002346519,
7.52769168467029));
#29814=CARTESIAN_POINT('Ctrl Pts',(-1.73950909287838,-2.56630936977627,
7.47531218016578));
#29815=CARTESIAN_POINT('Ctrl Pts',(-2.52300104774206,-1.80174953394315,
7.42293267566128));
#29816=CARTESIAN_POINT('Ctrl Pts',(-2.81153277662714,-0.881929231056029,
7.37055317115678));
#29817=CARTESIAN_POINT('Ctrl Pts',(-2.90036087316611,-0.598751062127826,
7.35442748646772));
#29818=CARTESIAN_POINT('Ctrl Pts',(-2.94227697960606,-0.300857412821767,
7.33830180177866));
#29819=CARTESIAN_POINT('Ctrl Pts',(-2.93998607517527,-0.0023358300504342,
7.3221761170896));
#29820=CARTESIAN_POINT('Ctrl Pts',(-2.93846014819028,-0.00170708260597003,
7.1778238829104));
#29821=CARTESIAN_POINT('Ctrl Pts',(-2.94044617033292,-0.369968033311824,
7.19769076223082));
#29822=CARTESIAN_POINT('Ctrl Pts',(-2.87617048586605,-0.737561088352721,
7.21755764155125));
#29823=CARTESIAN_POINT('Ctrl Pts',(-2.7424268268773,-1.07785126568817,7.23742452087168));
#29824=CARTESIAN_POINT('Ctrl Pts',(-2.38936683413567,-1.97615813457835,
7.28986962609539));
#29825=CARTESIAN_POINT('Ctrl Pts',(-1.55220665359259,-2.68419994513487,
7.34231473131909));
#29826=CARTESIAN_POINT('Ctrl Pts',(-0.60776265660645,-2.88327813520494,
7.3947598365428));
#29827=CARTESIAN_POINT('Ctrl Pts',(0.336681340379679,-3.082356325275,7.44720494176651));
#29828=CARTESIAN_POINT('Ctrl Pts',(1.38840915380886,-2.77247089485864,7.49965004699022));
#29829=CARTESIAN_POINT('Ctrl Pts',(2.07402481044015,-2.09310519028348,7.55209515221392));
#29830=CARTESIAN_POINT('Ctrl Pts',(2.75964046707144,-1.41373948570832,7.60454025743763));
#29831=CARTESIAN_POINT('Ctrl Pts',(3.07914396690482,-0.364893506974353,
7.65698536266134));
#29832=CARTESIAN_POINT('Ctrl Pts',(2.8887227491853,0.5813339228528,7.70943046788505));
#29833=CARTESIAN_POINT('Ctrl Pts',(2.69830153146578,1.52756135267996,7.76187557310876));
#29834=CARTESIAN_POINT('Ctrl Pts',(1.99795559619334,2.37117023360031,7.81432067833246));
#29835=CARTESIAN_POINT('Ctrl Pts',(1.10291949457769,2.73244155291697,7.86676578355617));
#29836=CARTESIAN_POINT('Ctrl Pts',(0.207883392962048,3.09371287223363,7.91921088877988));
#29837=CARTESIAN_POINT('Ctrl Pts',(-0.881842874996807,2.97264662994661,
7.97165599400359));
#29838=CARTESIAN_POINT('Ctrl Pts',(-1.67575975122609,2.42373627051487,8.0241010992273));
#29839=CARTESIAN_POINT('Ctrl Pts',(-2.45144772506959,1.88742928765845,8.07534202712166));
#29840=CARTESIAN_POINT('Ctrl Pts',(-2.94475435076587,0.942699847726619,
8.12658295501603));
#29841=CARTESIAN_POINT('Ctrl Pts',(-2.94656696235233,-0.000396508504380587,
8.1778238829104));
#29842=CARTESIAN_POINT('Origin',(0.,0.,0.));
#29843=CARTESIAN_POINT('',(-2.93787859032851,0.00118007037484616,9.3221761170896));
#29844=CARTESIAN_POINT('',(-2.93938212312892,0.00216771032458683,9.1778238829104));
#29845=CARTESIAN_POINT('',(-2.942,-3.60291088309151E-16,0.));
#29846=CARTESIAN_POINT('Ctrl Pts',(-2.93787859032851,0.00118007037484616,
9.3221761170896));
#29847=CARTESIAN_POINT('Ctrl Pts',(-2.93938225399168,0.408942454113454,
9.30018918916604));
#29848=CARTESIAN_POINT('Ctrl Pts',(-2.86009946358647,0.816145924853212,
9.27820226124249));
#29849=CARTESIAN_POINT('Ctrl Pts',(-2.69715242952518,1.18654365111784,9.25621533331894));
#29850=CARTESIAN_POINT('Ctrl Pts',(-2.30896336853928,2.06894293121702,9.20383582881443));
#29851=CARTESIAN_POINT('Ctrl Pts',(-1.44594933104186,2.74245624053358,9.15145632430993));
#29852=CARTESIAN_POINT('Ctrl Pts',(-0.495674163844965,2.9046210644708,9.09907681980542));
#29853=CARTESIAN_POINT('Ctrl Pts',(0.454601003351916,3.06678588840801,9.04669731530092));
#29854=CARTESIAN_POINT('Ctrl Pts',(1.49213730024827,2.7176022269659,8.99431781079641));
#29855=CARTESIAN_POINT('Ctrl Pts',(2.15099835280526,2.01388208359571,8.94193830629191));
#29856=CARTESIAN_POINT('Ctrl Pts',(2.80985940536224,1.31016194022553,8.88955880178741));
#29857=CARTESIAN_POINT('Ctrl Pts',(3.09004521357986,0.251905314927287,8.8371792972829));
#29858=CARTESIAN_POINT('Ctrl Pts',(2.86572951288042,-0.685645923387644,
8.7847997927784));
#29859=CARTESIAN_POINT('Ctrl Pts',(2.64141381218099,-1.62319716170258,8.73242028827389));
#29860=CARTESIAN_POINT('Ctrl Pts',(1.91259660256449,-2.44004301303419,8.68004078376939));
#29861=CARTESIAN_POINT('Ctrl Pts',(1.00657547791151,-2.76935400264746,8.62766127926488));
#29862=CARTESIAN_POINT('Ctrl Pts',(0.100554353258536,-3.09866499226073,
8.57528177476038));
#29863=CARTESIAN_POINT('Ctrl Pts',(-0.982670686430926,-2.94044112015566,
8.52290227025587));
#29864=CARTESIAN_POINT('Ctrl Pts',(-1.75664477537062,-2.36573767553097,
8.47052276575137));
#29865=CARTESIAN_POINT('Ctrl Pts',(-2.48731518632227,-1.82318876070292,
8.42107388286411));
#29866=CARTESIAN_POINT('Ctrl Pts',(-2.94237161798714,-0.909460413780999,
8.37162499997686));
#29867=CARTESIAN_POINT('Ctrl Pts',(-2.94622250669394,0.000937675328142526,
8.3221761170896));
#29868=CARTESIAN_POINT('Ctrl Pts',(-2.94656696235233,-0.000396508504380587,
8.1778238829104));
#29869=CARTESIAN_POINT('Ctrl Pts',(-2.94660955927376,-0.0225595585939061,
8.17902806023974));
#29870=CARTESIAN_POINT('Ctrl Pts',(-2.94638072162746,-0.0447217067897041,
8.18023223756908));
#29871=CARTESIAN_POINT('Ctrl Pts',(-2.94587773547044,-0.0668776312364038,
8.18143641489842));
#29872=CARTESIAN_POINT('Ctrl Pts',(-2.92397135898579,-1.03182669697942,
8.23388152012213));
#29873=CARTESIAN_POINT('Ctrl Pts',(-2.3820511215168,-1.98497035188899,8.28632662534583));
#29874=CARTESIAN_POINT('Ctrl Pts',(-1.5640421648278,-2.49728659914907,8.33877173056954));
#29875=CARTESIAN_POINT('Ctrl Pts',(-0.746033208138801,-3.00960284640916,
8.39121683579325));
#29876=CARTESIAN_POINT('Ctrl Pts',(0.348064467770205,-3.08109168601973,
8.44366194101695));
#29877=CARTESIAN_POINT('Ctrl Pts',(1.22578367546087,-2.6795750856597,8.49610704624066));
#29878=CARTESIAN_POINT('Ctrl Pts',(2.10350288315153,-2.27805848529968,8.54855215146437));
#29879=CARTESIAN_POINT('Ctrl Pts',(2.76484362262384,-1.40353644496905,8.60099725668809));
#29880=CARTESIAN_POINT('Ctrl Pts',(2.91212808132915,-0.44964238612263,8.65344236191179));
#29881=CARTESIAN_POINT('Ctrl Pts',(3.05941254003446,0.504251672723784,8.7058874671355));
#29882=CARTESIAN_POINT('Ctrl Pts',(2.69264071797276,1.537517750086,8.75833257235921));
#29883=CARTESIAN_POINT('Ctrl Pts',(1.97690123029279,2.18506974304829,8.81077767758291));
#29884=CARTESIAN_POINT('Ctrl Pts',(1.26116174261282,2.83262173601059,8.86322278280662));
#29885=CARTESIAN_POINT('Ctrl Pts',(0.196454589314577,3.09445964457298,8.91566788803033));
#29886=CARTESIAN_POINT('Ctrl Pts',(-0.737982063629216,2.8527269003752,8.96811299325404));
#29887=CARTESIAN_POINT('Ctrl Pts',(-1.672418716573,2.61099415617743,9.02055809847774));
#29888=CARTESIAN_POINT('Ctrl Pts',(-2.47658486916233,1.86569075921951,9.07300320370145));
#29889=CARTESIAN_POINT('Ctrl Pts',(-2.78851523225651,0.952287217651892,
9.12544830892515));
#29890=CARTESIAN_POINT('Ctrl Pts',(-2.89235416848512,0.648223031136026,
9.1429068335869));
#29891=CARTESIAN_POINT('Ctrl Pts',(-2.94164516567622,0.325530543639097,
9.16036535824865));
#29892=CARTESIAN_POINT('Ctrl Pts',(-2.93938212312892,0.00216771032458683,
9.1778238829104));
#29893=CARTESIAN_POINT('Origin',(0.,0.,0.));
#29894=CARTESIAN_POINT('',(-2.94242444587263,-0.00248500551853048,10.3221761170896));
#29895=CARTESIAN_POINT('',(-2.93989309841074,-0.00232834448912937,10.1778238829104));
#29896=CARTESIAN_POINT('',(-2.942,-3.60291088309151E-16,0.));
#29897=CARTESIAN_POINT('Ctrl Pts',(-2.94242444587263,-0.00248500551853048,
10.3221761170896));
#29898=CARTESIAN_POINT('Ctrl Pts',(-2.93565996783783,0.755676872330999,
10.2811328828597));
#29899=CARTESIAN_POINT('Ctrl Pts',(-2.63573211439715,1.5185652175411,10.2400896486299));
#29900=CARTESIAN_POINT('Ctrl Pts',(-2.10792737213773,2.05892622612073,10.1990464144));
#29901=CARTESIAN_POINT('Ctrl Pts',(-1.43434130141424,2.74853664338077,10.1466669098955));
#29902=CARTESIAN_POINT('Ctrl Pts',(-0.389613404070186,3.07571802003838,
10.094287405391));
#29903=CARTESIAN_POINT('Ctrl Pts',(0.557026464387836,2.89349108573471,10.0419079008865));
#29904=CARTESIAN_POINT('Ctrl Pts',(1.50366633284582,2.71126415143105,9.98952839638201));
#29905=CARTESIAN_POINT('Ctrl Pts',(2.35221817241779,2.01962890616612,9.9371488918775));
#29906=CARTESIAN_POINT('Ctrl Pts',(2.72164717416933,1.12921048240304,9.884769387373));
#29907=CARTESIAN_POINT('Ctrl Pts',(3.09107617592089,0.238792058639911,9.83238988286849));
#29908=CARTESIAN_POINT('Ctrl Pts',(2.981382339852,-0.85040954362138,9.78001037836398));
#29909=CARTESIAN_POINT('Ctrl Pts',(2.44180970997212,-1.64926869616342,9.72763087385948));
#29910=CARTESIAN_POINT('Ctrl Pts',(1.90223708009224,-2.44812784870545,9.67525136935497));
#29911=CARTESIAN_POINT('Ctrl Pts',(0.93278565640137,-2.95664455152821,9.62287186485046));
#29912=CARTESIAN_POINT('Ctrl Pts',(-0.031174037472469,-2.94644704900523,
9.57049236034596));
#29913=CARTESIAN_POINT('Ctrl Pts',(-0.995133731346301,-2.93624954648225,
9.51811285584146));
#29914=CARTESIAN_POINT('Ctrl Pts',(-1.9536016954031,-2.40733783861356,9.46573335133695));
#29915=CARTESIAN_POINT('Ctrl Pts',(-2.4761536351943,-1.5972393592383,9.41335384683245));
#29916=CARTESIAN_POINT('Ctrl Pts',(-2.77935810415337,-1.1271894741653,9.3829612702515));
#29917=CARTESIAN_POINT('Ctrl Pts',(-2.93580007289335,-0.56247072784923,
9.35256869367055));
#29918=CARTESIAN_POINT('Ctrl Pts',(-2.93787859032851,0.00118007037484616,
9.3221761170896));
#29919=CARTESIAN_POINT('Ctrl Pts',(-2.93938212312892,0.00216771032458683,
9.1778238829104));
#29920=CARTESIAN_POINT('Ctrl Pts',(-2.93484702512206,-0.645845798130107,
9.21281046347236));
#29921=CARTESIAN_POINT('Ctrl Pts',(-2.72327366311651,-1.29655137950586,
9.24779704403432));
#29922=CARTESIAN_POINT('Ctrl Pts',(-2.32875660055073,-1.80542543875765,
9.28278362459629));
#29923=CARTESIAN_POINT('Ctrl Pts',(-1.73737303215174,-2.56823086742229,
9.33522872981999));
#29924=CARTESIAN_POINT('Ctrl Pts',(-0.73491132175476,-3.01233803857425,
9.3876738350437));
#29925=CARTESIAN_POINT('Ctrl Pts',(0.227407657021308,-2.93784857599215,
9.44011894026741));
#29926=CARTESIAN_POINT('Ctrl Pts',(1.1897266357974,-2.86335911341005,9.49256404549111));
#29927=CARTESIAN_POINT('Ctrl Pts',(2.11190288295256,-2.27027301709385,9.54500915071482));
#29928=CARTESIAN_POINT('Ctrl Pts',(2.57885359588429,-1.42554607687093,9.59745425593853));
#29929=CARTESIAN_POINT('Ctrl Pts',(3.045804308816,-0.580819136648041,9.64989936116224));
#29930=CARTESIAN_POINT('Ctrl Pts',(3.05752948752431,0.515548647481566,9.70234446638595));
#29931=CARTESIAN_POINT('Ctrl Pts',(2.60875076544854,1.37006875926759,9.75478957160966));
#29932=CARTESIAN_POINT('Ctrl Pts',(2.15997204337277,2.22458887105361,9.80723467683336));
#29933=CARTESIAN_POINT('Ctrl Pts',(1.25068942051291,2.83726131049606,9.85967978205706));
#29934=CARTESIAN_POINT('Ctrl Pts',(0.290183858659324,2.93231357229399,9.91212488728077));
#29935=CARTESIAN_POINT('Ctrl Pts',(-0.67032170319427,3.02736583409193,9.96456999250448));
#29936=CARTESIAN_POINT('Ctrl Pts',(-1.68205020404159,2.60479791824536,10.0170150977282));
#29937=CARTESIAN_POINT('Ctrl Pts',(-2.28961248249041,1.85481470515708,10.0694602029519));
#29938=CARTESIAN_POINT('Ctrl Pts',(-2.708067067946,1.33826862311137,10.1055814296047));
#29939=CARTESIAN_POINT('Ctrl Pts',(-2.93479827488144,0.666407318052135,
10.1417026562576));
#29940=CARTESIAN_POINT('Ctrl Pts',(-2.93989309841074,-0.00232834448912937,
10.1778238829104));
#29941=CARTESIAN_POINT('Origin',(0.,0.,-1.84858989190501));
#29942=CARTESIAN_POINT('',(-2.3720921752204,-0.00200333509135781,10.651410108095));
#29943=CARTESIAN_POINT('',(-2.37533330856671,0.000645282184899808,10.848589891905));
#29944=CARTESIAN_POINT('',(-2.37175,-1.78696459712734E-13,-1.84858989190501));
#29945=CARTESIAN_POINT('',(-2.34668236863852,0.343918483395543,11.62825));
#29946=CARTESIAN_POINT('Ctrl Pts',(-2.3720921752204,-0.00200333509135741,
10.651410108095));
#29947=CARTESIAN_POINT('Ctrl Pts',(-2.37359839777753,-0.170820576644891,
10.6627463783696));
#29948=CARTESIAN_POINT('Ctrl Pts',(-2.28072670946568,-1.11802807678178,
10.7264621531488));
#29949=CARTESIAN_POINT('Ctrl Pts',(-1.0098707589218,-2.60498459805753,10.8425574324324));
#29950=CARTESIAN_POINT('Ctrl Pts',(1.61803174729613,-2.2773674076414,10.999695945946));
#29951=CARTESIAN_POINT('Ctrl Pts',(2.79127527466209,0.0946110570183949,
11.1568344594594));
#29952=CARTESIAN_POINT('Ctrl Pts',(1.46022534703361,2.38369320998594,11.313972972973));
#29953=CARTESIAN_POINT('Ctrl Pts',(-1.1878082887304,2.52773050943662,11.4711114864865));
#29954=CARTESIAN_POINT('Ctrl Pts',(-2.23349531079268,1.11623543008163,11.5758704954955));
#29955=CARTESIAN_POINT('Ctrl Pts',(-2.34668236863853,0.343918483395475,
11.62825));
#29956=CARTESIAN_POINT('',(-0.439445221994028,2.33068358199191,11.62825));
#29957=CARTESIAN_POINT('Origin',(0.,0.,11.62825));
#29958=CARTESIAN_POINT('Ctrl Pts',(-2.37533330856671,0.000645282184899929,
10.848589891905));
#29959=CARTESIAN_POINT('Ctrl Pts',(-2.37266626526946,-0.74297942345447,
10.8986961737085));
#29960=CARTESIAN_POINT('Ctrl Pts',(-1.5987407489101,-2.26979394046941,11.0012475607357));
#29961=CARTESIAN_POINT('Ctrl Pts',(0.989622905930635,-2.61290295808564,
11.1562440529866));
#29962=CARTESIAN_POINT('Ctrl Pts',(2.72902843688469,-0.61088887604173,11.3135793686578));
#29963=CARTESIAN_POINT('Ctrl Pts',(2.00599839187704,1.9449087769569,11.4709146843289));
#29964=CARTESIAN_POINT('Ctrl Pts',(0.328567026486064,2.47549058867235,11.5758048947763));
#29965=CARTESIAN_POINT('Ctrl Pts',(-0.439445221994061,2.3306835819919,11.62825));
#29966=CARTESIAN_POINT('Origin',(0.,0.,-1.84858989190501));
#29967=CARTESIAN_POINT('',(-2.36842744616303,0.000951336475574988,9.65141010809499));
#29968=CARTESIAN_POINT('',(-2.37005148067835,-0.00187703978340947,9.84858989190503));
#29969=CARTESIAN_POINT('',(-2.37175,-1.78696459712734E-13,-1.84858989190501));
#29970=CARTESIAN_POINT('Ctrl Pts',(-2.36842744616303,0.000951336475575049,
9.65141010809499));
#29971=CARTESIAN_POINT('Ctrl Pts',(-2.36675180927421,-0.453446617531184,
9.68180268467594));
#29972=CARTESIAN_POINT('Ctrl Pts',(-2.02327622703562,-1.69331275929724,
9.76457476576139));
#29973=CARTESIAN_POINT('Ctrl Pts',(-0.0295588149451427,-2.79350652787453,
9.89972635135136));
#29974=CARTESIAN_POINT('Ctrl Pts',(2.31506703223917,-1.56365490661018,10.0568648648649));
#29975=CARTESIAN_POINT('Ctrl Pts',(2.58036243233743,1.07058768363104,10.2140033783784));
#29976=CARTESIAN_POINT('Ctrl Pts',(0.528133174514654,2.74331293137788,10.3711418918919));
#29977=CARTESIAN_POINT('Ctrl Pts',(-1.81626974066498,2.00910742659655,10.5169441351307));
#29978=CARTESIAN_POINT('Ctrl Pts',(-2.36663886088356,0.609203474490441,
10.6103668738651));
#29979=CARTESIAN_POINT('Ctrl Pts',(-2.3720921752204,-0.00200333509135741,
10.651410108095));
#29980=CARTESIAN_POINT('Ctrl Pts',(-2.37005148067835,-0.0018770397834093,
9.84858989190503));
#29981=CARTESIAN_POINT('Ctrl Pts',(-2.37190764427919,-0.245513112411714,
9.8649137704759));
#29982=CARTESIAN_POINT('Ctrl Pts',(-2.22599738542921,-1.26973141402768,
9.93368275427047));
#29983=CARTESIAN_POINT('Ctrl Pts',(-0.757654725048104,-2.69016151139635,
10.0548968432888));
#29984=CARTESIAN_POINT('Ctrl Pts',(1.83027666927001,-2.11210170665972,10.2122321589599));
#29985=CARTESIAN_POINT('Ctrl Pts',(2.77060484795253,0.367287133540841,10.369567474631));
#29986=CARTESIAN_POINT('Ctrl Pts',(1.21665350181368,2.51610800548609,10.5269027903021));
#29987=CARTESIAN_POINT('Ctrl Pts',(-1.43234772356642,2.39972494583597,10.6842381059733));
#29988=CARTESIAN_POINT('Ctrl Pts',(-2.35921176770024,0.848280000432971,
10.7914671398409));
#29989=CARTESIAN_POINT('Ctrl Pts',(-2.37545779881228,0.0353556381482985,
10.8462510684848));
#29990=CARTESIAN_POINT('Ctrl Pts',(-2.37533330856671,0.000645282184899929,
10.848589891905));
#29991=CARTESIAN_POINT('Origin',(0.,0.,-1.84858989190501));
#29992=CARTESIAN_POINT('',(-2.37515405515002,0.000755925037124906,8.65141010809499));
#29993=CARTESIAN_POINT('',(-2.36963954810708,0.00174754145538428,8.84858989190503));
#29994=CARTESIAN_POINT('',(-2.37175,-1.78696459712734E-13,-1.84858989190501));
#29995=CARTESIAN_POINT('Ctrl Pts',(-2.37515405515002,0.00075592503712492,
8.65141010809499));
#29996=CARTESIAN_POINT('Ctrl Pts',(-2.37204958700235,-0.733179040239741,
8.70085899098224));
#29997=CARTESIAN_POINT('Ctrl Pts',(-1.61660279875904,-2.25007474146859,
8.80268737837401));
#29998=CARTESIAN_POINT('Ctrl Pts',(0.954326572136137,-2.62560372673677,
8.95689527027026));
#29999=CARTESIAN_POINT('Ctrl Pts',(2.71697669134881,-0.650055649344734,
9.11403378378378));
#30000=CARTESIAN_POINT('Ctrl Pts',(2.03934512373477,1.90934627218937,9.2711722972973));
#30001=CARTESIAN_POINT('Ctrl Pts',(-0.469944521571767,2.75384968723896,
9.42831081081079));
#30002=CARTESIAN_POINT('Ctrl Pts',(-2.15345863304216,1.44000181080629,9.55505674774338));
#30003=CARTESIAN_POINT('Ctrl Pts',(-2.36963965360463,0.329676840769313,
9.62942318017144));
#30004=CARTESIAN_POINT('Ctrl Pts',(-2.36842744616303,0.000951336475575049,
9.65141010809499));
#30005=CARTESIAN_POINT('Ctrl Pts',(-2.36963954810708,0.00174754145538407,
8.84858989190503));
#30006=CARTESIAN_POINT('Ctrl Pts',(-2.36598349144566,-0.520661037292834,
8.88357647246699));
#30007=CARTESIAN_POINT('Ctrl Pts',(-1.9397431197991,-1.83158688452099,8.97100815825266));
#30008=CARTESIAN_POINT('Ctrl Pts',(0.215690902196592,-2.78647992051942,
9.11088494926201));
#30009=CARTESIAN_POINT('Ctrl Pts',(2.4459813653409,-1.35209655994371,9.26822026493315));
#30010=CARTESIAN_POINT('Ctrl Pts',(2.47433880171217,1.29947749716991,9.42555558060427));
#30011=CARTESIAN_POINT('Ctrl Pts',(0.275231669725872,2.78123058171878,9.58289089627539));
#30012=CARTESIAN_POINT('Ctrl Pts',(-1.91777323438188,1.86527979947427,9.72390233337565));
#30013=CARTESIAN_POINT('Ctrl Pts',(-2.36594419049973,0.537237102851684,
9.81246866525219));
#30014=CARTESIAN_POINT('Ctrl Pts',(-2.37005148067835,-0.0018770397834093,
9.84858989190503));
#30015=CARTESIAN_POINT('Origin',(0.,0.,-1.84858989190501));
#30016=CARTESIAN_POINT('',(-2.37012643568897,-0.00188307441280249,7.65141010809499));
#30017=CARTESIAN_POINT('',(-2.37543174471759,-0.000319652972777529,7.84858989190503));
#30018=CARTESIAN_POINT('',(-2.37175,-1.78696459712734E-13,-1.84858989190501));
#30019=CARTESIAN_POINT('Ctrl Pts',(-2.37012643568897,-0.00188307441280247,
7.65141010809499));
#30020=CARTESIAN_POINT('Ctrl Pts',(-2.37197329244753,-0.242542001652036,
7.66753579278404));
#30021=CARTESIAN_POINT('Ctrl Pts',(-2.22842022339473,-1.26275955622086,
7.7360409819776));
#30022=CARTESIAN_POINT('Ctrl Pts',(-0.770711640749916,-2.68524440462409,
7.85692567567567));
#30023=CARTESIAN_POINT('Ctrl Pts',(1.81639251383808,-2.12255793467458,8.01406418918919));
#30024=CARTESIAN_POINT('Ctrl Pts',(2.77208469636934,0.346526200869026,8.1712027027027));
#30025=CARTESIAN_POINT('Ctrl Pts',(1.23799993580832,2.50437418705365,8.32834121621622));
#30026=CARTESIAN_POINT('Ctrl Pts',(-1.40800742257503,2.4128922603655,8.48547972972973));
#30027=CARTESIAN_POINT('Ctrl Pts',(-2.35469744140074,0.865004378788607,
8.59316936035599));
#30028=CARTESIAN_POINT('Ctrl Pts',(-2.37533804356255,0.0442530790537146,
8.64847948647774));
#30029=CARTESIAN_POINT('Ctrl Pts',(-2.37515405515002,0.00075592503712492,
8.65141010809499));
#30030=CARTESIAN_POINT('Ctrl Pts',(-2.37543174471759,-0.000319652972777509,
7.84858989190503));
#30031=CARTESIAN_POINT('Ctrl Pts',(-2.37546608504675,-0.0181868229420618,
7.84979406923436));
#30032=CARTESIAN_POINT('Ctrl Pts',(-2.36724692977477,-0.814184073087101,
7.9034433517874));
#30033=CARTESIAN_POINT('Ctrl Pts',(-1.48345697628832,-2.36861723168749,
8.00953773956416));
#30034=CARTESIAN_POINT('Ctrl Pts',(1.16262680634646,-2.54151354917186,8.16687305523529));
#30035=CARTESIAN_POINT('Ctrl Pts',(2.76208455499713,-0.426475157784177,
8.3242083709064));
#30036=CARTESIAN_POINT('Ctrl Pts',(1.8750440359881,2.07248692819523,8.48154368657753));
#30037=CARTESIAN_POINT('Ctrl Pts',(-0.699958537943023,2.7057439570526,8.63887900224866));
#30038=CARTESIAN_POINT('Ctrl Pts',(-2.21235813584821,1.30404785948979,8.76122773735781));
#30039=CARTESIAN_POINT('Ctrl Pts',(-2.37146394347132,0.262432721575661,
8.83113136724327));
#30040=CARTESIAN_POINT('Ctrl Pts',(-2.36963954810708,0.00174754145538407,
8.84858989190503));
#30041=CARTESIAN_POINT('Origin',(0.,0.,-1.84858989190501));
#30042=CARTESIAN_POINT('',(-2.36973441944585,0.0017659640348839,6.65141010809499));
#30043=CARTESIAN_POINT('',(-2.36889628024144,-0.00137619754296547,6.84858989190503));
#30044=CARTESIAN_POINT('',(-2.37175,-1.78696459712734E-13,-1.84858989190501));
#30045=CARTESIAN_POINT('Ctrl Pts',(-2.36973441944585,0.00176596403488379,
6.65141010809499));
#30046=CARTESIAN_POINT('Ctrl Pts',(-2.36600087280351,-0.523508321396127,
6.68659209909035));
#30047=CARTESIAN_POINT('Ctrl Pts',(-1.93625564677593,-1.83636884117464,
6.77415359459022));
#30048=CARTESIAN_POINT('Ctrl Pts',(0.222416181733502,-2.78479173243988,
6.91409459459459));
#30049=CARTESIAN_POINT('Ctrl Pts',(2.4466042959518,-1.34857753576241,7.0712331081081));
#30050=CARTESIAN_POINT('Ctrl Pts',(2.47334911304448,1.29887571249989,7.22837162162162));
#30051=CARTESIAN_POINT('Ctrl Pts',(0.278629494786153,2.77973012269657,7.38551013513513));
#30052=CARTESIAN_POINT('Ctrl Pts',(-1.91543890246215,1.86818192765693,7.52652296395959));
#30053=CARTESIAN_POINT('Ctrl Pts',(-2.36597432596829,0.539167154048567,
7.61515628827954));
#30054=CARTESIAN_POINT('Ctrl Pts',(-2.37012643568897,-0.00188307441280247,
7.65141010809499));
#30055=CARTESIAN_POINT('Ctrl Pts',(-2.36889628024144,-0.0013761975429653,
6.84858989190503));
#30056=CARTESIAN_POINT('Ctrl Pts',(-2.37049735026751,-0.298256860301772,
6.86845677122545));
#30057=CARTESIAN_POINT('Ctrl Pts',(-2.18189218700624,-1.37689100842058,
6.94076875576958));
#30058=CARTESIAN_POINT('Ctrl Pts',(-0.57644849505612,-2.73472106868152,
7.06552584553741));
#30059=CARTESIAN_POINT('Ctrl Pts',(1.96716344393165,-1.98526073259378,7.22286116120855));
#30060=CARTESIAN_POINT('Ctrl Pts',(2.73988515609665,0.551381466653972,7.38019647687966));
#30061=CARTESIAN_POINT('Ctrl Pts',(1.04609303646807,2.5916561403346,7.53753179255079));
#30062=CARTESIAN_POINT('Ctrl Pts',(-1.56924738212969,2.3010974504224,7.69366293089257));
#30063=CARTESIAN_POINT('Ctrl Pts',(-2.3739704729535,0.759975650525201,7.79734896401065));
#30064=CARTESIAN_POINT('Ctrl Pts',(-2.37543174471759,-0.000319652972777509,
7.84858989190503));
#30065=CARTESIAN_POINT('Origin',(0.,0.,-1.84858989190501));
#30066=CARTESIAN_POINT('',(-2.37533640146812,-0.000487534612837604,5.65141010809499));
#30067=CARTESIAN_POINT('',(-2.3710171167516,0.00204493508413422,5.84858989190502));
#30068=CARTESIAN_POINT('',(-2.37175,-1.78696459712734E-13,-1.84858989190501));
#30069=CARTESIAN_POINT('Ctrl Pts',(-2.37533640146812,-0.000487534612837498,
5.65141010809499));
#30070=CARTESIAN_POINT('Ctrl Pts',(-2.3754150982357,-0.0280706202968775,
5.65326890089215));
#30071=CARTESIAN_POINT('Ctrl Pts',(-2.36258260410634,-0.832851216236821,
5.70750719819383));
#30072=CARTESIAN_POINT('Ctrl Pts',(-1.45646562934828,-2.38395507960311,
5.81412499999999));
#30073=CARTESIAN_POINT('Ctrl Pts',(1.18715361157964,-2.5288733170224,5.97126351351352));
#30074=CARTESIAN_POINT('Ctrl Pts',(2.76451839080433,-0.402457473451116,
6.12840202702702));
#30075=CARTESIAN_POINT('Ctrl Pts',(1.8589019956498,2.08542976904401,6.28554054054054));
#30076=CARTESIAN_POINT('Ctrl Pts',(-0.716306714602523,2.70026640197657,
6.44267905405405));
#30077=CARTESIAN_POINT('Ctrl Pts',(-2.21563200675447,1.29517183256302,6.5646355765722));
#30078=CARTESIAN_POINT('Ctrl Pts',(-2.37155943608083,0.258528340584143,
6.63421259458585));
#30079=CARTESIAN_POINT('Ctrl Pts',(-2.36973441944585,0.00176596403488379,
6.65141010809499));
#30080=CARTESIAN_POINT('Ctrl Pts',(-2.3710171167516,0.00204493508413416,
5.84858989190502));
#30081=CARTESIAN_POINT('Ctrl Pts',(-2.36609071130836,-0.572418580286349,
5.88711947321653));
#30082=CARTESIAN_POINT('Ctrl Pts',(-1.86927748327345,-1.93646185988882,
5.97809415975175));
#30083=CARTESIAN_POINT('Ctrl Pts',(0.401163844498212,-2.76587414046649,
6.12151395151068));
#30084=CARTESIAN_POINT('Ctrl Pts',(2.53076037597685,-1.18585163930103,6.2788492671818));
#30085=CARTESIAN_POINT('Ctrl Pts',(2.38210248511723,1.46170446446183,6.43618458285292));
#30086=CARTESIAN_POINT('Ctrl Pts',(0.0890157606711408,2.793397283841,6.59351989852405));
#30087=CARTESIAN_POINT('Ctrl Pts',(-1.98453634187054,1.75978107224967,6.73098833487474));
#30088=CARTESIAN_POINT('Ctrl Pts',(-2.36627080393209,0.485456441931073,
6.81601166600174));
#30089=CARTESIAN_POINT('Ctrl Pts',(-2.36889628024144,-0.0013761975429653,
6.84858989190503));
#30090=CARTESIAN_POINT('Origin',(0.,0.,-1.84858989190501));
#30091=CARTESIAN_POINT('',(-2.36864740940268,-0.0011676470311218,4.65141010809498));
#30092=CARTESIAN_POINT('',(-2.37471653528189,-0.00117837014130401,4.84858989190502));
#30093=CARTESIAN_POINT('',(-2.37175,-1.78696459712734E-13,-1.84858989190501));
#30094=CARTESIAN_POINT('Ctrl Pts',(-2.36864740940268,-0.00116764703112199,
4.65141010809498));
#30095=CARTESIAN_POINT('Ctrl Pts',(-2.37007090104248,-0.313795660845675,
4.67232520719846));
#30096=CARTESIAN_POINT('Ctrl Pts',(-2.16810014725707,-1.40760004764448,
4.74561981080643));
#30097=CARTESIAN_POINT('Ctrl Pts',(-0.525482821607704,-2.74379331497496,
4.87129391891892));
#30098=CARTESIAN_POINT('Ctrl Pts',(2.00035639160479,-1.95015595724574,5.02843243243243));
#30099=CARTESIAN_POINT('Ctrl Pts',(2.72955454106374,0.595034417816705,5.18557094594594));
#30100=CARTESIAN_POINT('Ctrl Pts',(1.0071746643292,2.60578839251754,5.34270945945947));
#30101=CARTESIAN_POINT('Ctrl Pts',(-1.58873507575841,2.28002578161798,5.49798918017579));
#30102=CARTESIAN_POINT('Ctrl Pts',(-2.37319747737008,0.7492017916888,5.60088939638765));
#30103=CARTESIAN_POINT('Ctrl Pts',(-2.37533640146812,-0.000487534612837498,
5.65141010809499));
#30104=CARTESIAN_POINT('Ctrl Pts',(-2.37471653528189,-0.00117837014130423,
4.84858989190502));
#30105=CARTESIAN_POINT('Ctrl Pts',(-2.37515017179056,-0.0716719020310164,
4.85333706998391));
#30106=CARTESIAN_POINT('Ctrl Pts',(-2.34054813360425,-0.920521113001663,
4.91052935328651));
#30107=CARTESIAN_POINT('Ctrl Pts',(-1.32208186928512,-2.46233460804071,
5.02016674181281));
#30108=CARTESIAN_POINT('Ctrl Pts',(1.32964132424929,-2.45826079574207,5.17750205748394));
#30109=CARTESIAN_POINT('Ctrl Pts',(2.78438780839412,-0.241198514719961,
5.33483737315506));
#30110=CARTESIAN_POINT('Ctrl Pts',(1.73255804842731,2.19299676239354,5.49217268882618));
#30111=CARTESIAN_POINT('Ctrl Pts',(-0.878964234485193,2.65300095467984,
5.64950800449731));
#30112=CARTESIAN_POINT('Ctrl Pts',(-2.25346115704322,1.19692341827648,5.76831373885692));
#30113=CARTESIAN_POINT('Ctrl Pts',(-2.37279636039799,0.20952086689332,5.83467436799283));
#30114=CARTESIAN_POINT('Ctrl Pts',(-2.3710171167516,0.00204493508413416,
5.84858989190502));
#30115=CARTESIAN_POINT('Origin',(0.,0.,-1.84858989190501));
#30116=CARTESIAN_POINT('',(-2.37165914320747,0.00205379600805495,3.65141010809498));
#30117=CARTESIAN_POINT('',(-2.36819322153198,-0.000653453332863235,3.84858989190502));
#30118=CARTESIAN_POINT('',(-2.37175,-1.78696459712734E-13,-1.84858989190501));
#30119=CARTESIAN_POINT('Ctrl Pts',(-2.37165914320747,0.0020537960080548,
3.65141010809498));
#30120=CARTESIAN_POINT('Ctrl Pts',(-2.36638740749304,-0.593495286532831,
3.69138151350476));
#30121=CARTESIAN_POINT('Ctrl Pts',(-1.83931642681201,-1.97778866762885,
3.78373242341905));
#30122=CARTESIAN_POINT('Ctrl Pts',(0.47257542983782,-2.75339906613161,3.92846283783783));
#30123=CARTESIAN_POINT('Ctrl Pts',(2.55822296043148,-1.12251023841371,4.08560135135135));
#30124=CARTESIAN_POINT('Ctrl Pts',(2.34617571991457,1.51657292659299,4.24273986486486));
#30125=CARTESIAN_POINT('Ctrl Pts',(0.0268861606557786,2.79353021925399,
4.39987837837838));
#30126=CARTESIAN_POINT('Ctrl Pts',(-2.00464048744226,1.72543877128143,4.53610179278842));
#30127=CARTESIAN_POINT('Ctrl Pts',(-2.36650592693501,0.469145905762286,
4.61994570269395));
#30128=CARTESIAN_POINT('Ctrl Pts',(-2.36864740940268,-0.00116764703112199,
4.65141010809498));
#30129=CARTESIAN_POINT('Ctrl Pts',(-2.36819322153198,-0.000653453332863235,
3.84858989190502));
#30130=CARTESIAN_POINT('Ctrl Pts',(-2.36907284142701,-0.350739660290616,
3.871999771975));
#30131=CARTESIAN_POINT('Ctrl Pts',(-2.13320735842129,-1.48399610964751,
3.94785475726868));
#30132=CARTESIAN_POINT('Ctrl Pts',(-0.392663608746353,-2.76709368867159,
4.07615484778607));
#30133=CARTESIAN_POINT('Ctrl Pts',(2.09526330020315,-1.8495577562663,4.23349016345719));
#30134=CARTESIAN_POINT('Ctrl Pts',(2.69698125586998,0.732996791565816,4.39082547912832));
#30135=CARTESIAN_POINT('Ctrl Pts',(0.870808554093777,2.65568911080063,4.54816079479944));
#30136=CARTESIAN_POINT('Ctrl Pts',(-1.66053522846232,2.20178445767042,4.70074893239168));
#30137=CARTESIAN_POINT('Ctrl Pts',(-2.37035951259304,0.707115123883991,
4.8008919647602));
#30138=CARTESIAN_POINT('Ctrl Pts',(-2.37471653528189,-0.00117837014130423,
4.84858989190502));
#30139=CARTESIAN_POINT('Origin',(0.,0.,-1.84858989190501));
#30140=CARTESIAN_POINT('',(-2.37406517885066,-0.00153607482357252,2.65141010809498));
#30141=CARTESIAN_POINT('',(-2.37255724078598,0.00199178475905649,2.84858989190502));
#30142=CARTESIAN_POINT('',(-2.37175,-1.78696459712734E-13,-1.84858989190501));
#30143=CARTESIAN_POINT('Ctrl Pts',(-2.37406517885066,-0.00153607482357281,
2.65141010809498));
#30144=CARTESIAN_POINT('Ctrl Pts',(-2.37481281249436,-0.100330398866114,
2.65805831530656));
#30145=CARTESIAN_POINT('Ctrl Pts',(-2.32469515905834,-0.976735840432517,
2.71708602702265));
#30146=CARTESIAN_POINT('Ctrl Pts',(-1.23560715428754,-2.50555554774625,
2.82849324324324));
#30147=CARTESIAN_POINT('Ctrl Pts',(1.41031161531747,-2.41154623133624,2.98563175675675));
#30148=CARTESIAN_POINT('Ctrl Pts',(2.78954424185296,-0.151581281506301,
3.14277027027027));
#30149=CARTESIAN_POINT('Ctrl Pts',(1.66331845351111,2.24452793077997,3.29990878378378));
#30150=CARTESIAN_POINT('Ctrl Pts',(-0.956834235921451,2.62469088021855,
3.45704729729729));
#30151=CARTESIAN_POINT('Ctrl Pts',(-2.26971028444252,1.15040938517441,3.57421440540103));
#30152=CARTESIAN_POINT('Ctrl Pts',(-2.37329561854466,0.186926755969883,
3.63900200900026));
#30153=CARTESIAN_POINT('Ctrl Pts',(-2.37165914320747,0.0020537960080548,
3.65141010809498));
#30154=CARTESIAN_POINT('Ctrl Pts',(-2.37255724078598,0.00199178475905658,
2.84858989190502));
#30155=CARTESIAN_POINT('Ctrl Pts',(-2.36697397570993,-0.624252704055323,
2.89066247396608));
#30156=CARTESIAN_POINT('Ctrl Pts',(-1.79321255273579,-2.04018921676783,
2.98518016125086));
#30157=CARTESIAN_POINT('Ctrl Pts',(0.584848394656438,-2.73293698550247,
3.13214295375933));
#30158=CARTESIAN_POINT('Ctrl Pts',(2.60425579784155,-1.01431944186932,3.28947826943046));
#30159=CARTESIAN_POINT('Ctrl Pts',(2.27924634057658,1.61741407950708,3.44681358510158));
#30160=CARTESIAN_POINT('Ctrl Pts',(-0.0975982492034651,2.79311059143494,
3.6041489007727));
#30161=CARTESIAN_POINT('Ctrl Pts',(-2.04600507844241,1.65356799864077,3.73807433637385));
#30162=CARTESIAN_POINT('Ctrl Pts',(-2.36710223082098,0.433557734928271,
3.81955466675129));
#30163=CARTESIAN_POINT('Ctrl Pts',(-2.36819322153198,-0.000653453332863235,
3.84858989190502));
#30164=CARTESIAN_POINT('Origin',(0.,0.,-1.84858989190501));
#30165=CARTESIAN_POINT('',(-2.36804188512505,-0.000112073902353324,1.65141010809498));
#30166=CARTESIAN_POINT('',(-2.37344137975612,-0.00178937704920473,1.84858989190502));
#30167=CARTESIAN_POINT('',(-2.37175,-1.78696459712734E-13,-1.84858989190501));
#30168=CARTESIAN_POINT('Ctrl Pts',(-2.36804188512505,-0.000112073902353224,
1.65141010809498));
#30169=CARTESIAN_POINT('Ctrl Pts',(-2.36821023678956,-0.384577180330964,
1.67711462161287));
#30170=CARTESIAN_POINT('Ctrl Pts',(-2.09930421630608,-1.55226751145704,
1.75519863963526));
#30171=CARTESIAN_POINT('Ctrl Pts',(-0.275973625536248,-2.77999224892802,
1.88566216216216));
#30172=CARTESIAN_POINT('Ctrl Pts',(2.16802781286073,-1.76187209738162,2.04280067567567));
#30173=CARTESIAN_POINT('Ctrl Pts',(2.66479327803676,0.838697048159531,2.19993918918919));
#30174=CARTESIAN_POINT('Ctrl Pts',(0.76814623510466,2.68597898024514,2.3570777027027));
#30175=CARTESIAN_POINT('Ctrl Pts',(-1.70898688612053,2.14473275169325,2.50756800900463));
#30176=CARTESIAN_POINT('Ctrl Pts',(-2.36892240045369,0.678044518839718,
2.60567881080206));
#30177=CARTESIAN_POINT('Ctrl Pts',(-2.37406517885066,-0.00153607482357281,
2.65141010809498));
#30178=CARTESIAN_POINT('Ctrl Pts',(-2.37344137975612,-0.00178937704920463,
1.84858989190502));
#30179=CARTESIAN_POINT('Ctrl Pts',(-2.37447812169567,-0.12506848067989,
1.85688007073346));
#30180=CARTESIAN_POINT('Ctrl Pts',(-2.31006431944847,-1.02714724785255,
1.91761535478561));
#30181=CARTESIAN_POINT('Ctrl Pts',(-1.15481219883121,-2.54507342378116,
2.03079574406147));
#30182=CARTESIAN_POINT('Ctrl Pts',(1.49072764255621,-2.36404822464922,2.18813105973259));
#30183=CARTESIAN_POINT('Ctrl Pts',(2.79427705549031,-0.0548463935276453,
2.34546637540372));
#30184=CARTESIAN_POINT('Ctrl Pts',(1.5823475414007,2.30372918060613,2.50280169107483));
#30185=CARTESIAN_POINT('Ctrl Pts',(-1.05405113312049,2.58842974112365,2.66013700674597));
#30186=CARTESIAN_POINT('Ctrl Pts',(-2.29031280961247,1.08993341565411,2.77539974035602));
#30187=CARTESIAN_POINT('Ctrl Pts',(-2.37393373216083,0.15638533864836,2.83821736874238));
#30188=CARTESIAN_POINT('Ctrl Pts',(-2.37255724078598,0.00199178475905658,
2.84858989190502));
#30189=CARTESIAN_POINT('Origin',(0.,0.,-1.84858989190501));
#30190=CARTESIAN_POINT('',(-2.37366757034868,0.00184471646948807,0.651410108094983));
#30191=CARTESIAN_POINT('',(-2.36802324146013,0.000186122305323028,0.848589891905023));
#30192=CARTESIAN_POINT('',(-2.37175,-1.78696459712734E-13,-1.84858989190501));
#30193=CARTESIAN_POINT('Ctrl Pts',(-2.37366757034868,0.001844716469488,
0.651410108094984));
#30194=CARTESIAN_POINT('Ctrl Pts',(-2.36827887140227,-0.663567421798888,
0.696170927919177));
#30195=CARTESIAN_POINT('Ctrl Pts',(-1.73206830317985,-2.11713322740477,
0.793311252247876));
#30196=CARTESIAN_POINT('Ctrl Pts',(0.718910407331439,-2.69944634094777,
0.942831081081078));
#30197=CARTESIAN_POINT('Ctrl Pts',(2.64899289676255,-0.887370898887054,
1.09996959459459));
#30198=CARTESIAN_POINT('Ctrl Pts',(2.19990031581894,1.72195501972256,1.25710810810811));
#30199=CARTESIAN_POINT('Ctrl Pts',(-0.225079684819506,2.78455874530281,
1.41424662162162));
#30200=CARTESIAN_POINT('Ctrl Pts',(-2.08428517335687,1.58152664346482,1.54568062161725));
#30201=CARTESIAN_POINT('Ctrl Pts',(-2.36786717732013,0.39886856587965,1.62473511710837));
#30202=CARTESIAN_POINT('Ctrl Pts',(-2.36804188512505,-0.000112073902353224,
1.65141010809498));
#30203=CARTESIAN_POINT('Ctrl Pts',(-2.36802324146013,0.000186122305323062,
0.848589891905023));
#30204=CARTESIAN_POINT('Ctrl Pts',(-2.36776001721126,-0.402962357372647,
0.87554277272455));
#30205=CARTESIAN_POINT('Ctrl Pts',(-2.0797505690667,-1.59092671500009,0.954940758767785));
#30206=CARTESIAN_POINT('Ctrl Pts',(-0.207121339063888,-2.78711087979173,
1.08678385003473));
#30207=CARTESIAN_POINT('Ctrl Pts',(2.21401803077907,-1.70561830406782,1.24411916570585));
#30208=CARTESIAN_POINT('Ctrl Pts',(2.64205485235054,0.911349150745493,1.40145448137697));
#30209=CARTESIAN_POINT('Ctrl Pts',(0.691640660298454,2.70787919402874,1.5587897970481));
#30210=CARTESIAN_POINT('Ctrl Pts',(-1.74582592441822,2.10050088985172,1.70783493389078));
#30211=CARTESIAN_POINT('Ctrl Pts',(-2.36791951286044,0.654816452515466,
1.80443496550976));
#30212=CARTESIAN_POINT('Ctrl Pts',(-2.37344137975612,-0.00178937704920463,
1.84858989190502));
#30213=CARTESIAN_POINT('Origin',(0.,0.,11.5));
#30214=CARTESIAN_POINT('',(-2.86997293948595,0.000709208322249463,11.1339652973708));
#30215=CARTESIAN_POINT('Ctrl Pts',(-0.439445221994061,2.3306835819919,11.62825));
#30216=CARTESIAN_POINT('Ctrl Pts',(-0.359483020814685,2.34931149018937,
11.6247602761445));
#30217=CARTESIAN_POINT('Ctrl Pts',(-0.27871400731898,2.36341693162049,11.6212847858384));
#30218=CARTESIAN_POINT('Ctrl Pts',(-0.197463562604575,2.37318447045242,
11.6178187998135));
#30219=CARTESIAN_POINT('Ctrl Pts',(-0.114065564321399,2.38321017787593,
11.614261203328));
#30220=CARTESIAN_POINT('Ctrl Pts',(-0.0301595928545948,2.38866567182183,
11.6107136201843));
#30221=CARTESIAN_POINT('Ctrl Pts',(0.0539178478306465,2.38969830818771,
11.6071709361129));
#30222=CARTESIAN_POINT('Ctrl Pts',(0.0934462943689916,2.39018379527021,
11.6055053668855));
#30223=CARTESIAN_POINT('Ctrl Pts',(0.133012786809523,2.38969093626847,11.6038408805234));
#30224=CARTESIAN_POINT('Ctrl Pts',(0.172582728329755,2.38823118545469,11.6021769455617));
#30225=CARTESIAN_POINT('Ctrl Pts',(0.196983674678661,2.38733102488025,11.6011508741002));
#30226=CARTESIAN_POINT('Ctrl Pts',(0.221385934120707,2.38606314465001,11.6001250123152));
#30227=CARTESIAN_POINT('Ctrl Pts',(0.24578137026875,2.38442977721171,11.5990992355836));
#30228=CARTESIAN_POINT('Ctrl Pts',(0.261730484740349,2.38336192320454,11.5984286088969));
#30229=CARTESIAN_POINT('Ctrl Pts',(0.277677591321838,2.38213767553654,11.597757980196));
#30230=CARTESIAN_POINT('Ctrl Pts',(0.293603734342933,2.38075929535175,11.5970880163414));
#30231=CARTESIAN_POINT('Ctrl Pts',(0.379341030417818,2.37333888038685,11.5934813119885));
#30232=CARTESIAN_POINT('Ctrl Pts',(0.464583014225527,2.36144918428767,11.5898891320915));
#30233=CARTESIAN_POINT('Ctrl Pts',(0.548977057540434,2.34525221307984,11.5863062427765));
#30234=CARTESIAN_POINT('Ctrl Pts',(0.63410785152571,2.32891384410355,11.5826920752337));
#30235=CARTESIAN_POINT('Ctrl Pts',(0.718376786391574,2.30819252148602,11.5790873611926));
#30236=CARTESIAN_POINT('Ctrl Pts',(0.801421129360431,2.28320149524268,11.5754867285058));
#30237=CARTESIAN_POINT('Ctrl Pts',(0.851520069054253,2.26812492443856,11.5733145410529));
#30238=CARTESIAN_POINT('Ctrl Pts',(0.901173245121242,2.25149340059607,11.5711438389925));
#30239=CARTESIAN_POINT('Ctrl Pts',(0.950298631716725,2.23332291784394,11.5689734428101));
#30240=CARTESIAN_POINT('Ctrl Pts',(0.963508179039198,2.22843697457875,11.5683898351671));
#30241=CARTESIAN_POINT('Ctrl Pts',(0.976678902975083,2.22343988211883,11.5678062771152));
#30242=CARTESIAN_POINT('Ctrl Pts',(0.989796896482515,2.2183369213822,11.5672232951128));
#30243=CARTESIAN_POINT('Ctrl Pts',(1.0715488401239,2.18653503351653,11.5635901242489));
#30244=CARTESIAN_POINT('Ctrl Pts',(1.15137916677557,2.15057972741051,11.5599737688071));
#30245=CARTESIAN_POINT('Ctrl Pts',(1.22892868995964,2.11061806082819,11.5563689172299));
#30246=CARTESIAN_POINT('Ctrl Pts',(1.30609743699769,2.07085261014462,11.5527817658451));
#30247=CARTESIAN_POINT('Ctrl Pts',(1.38100867140758,2.02711976610499,11.5492060056319));
#30248=CARTESIAN_POINT('Ctrl Pts',(1.45329568150197,1.97951483102432,11.5456364028898));
#30249=CARTESIAN_POINT('Ctrl Pts',(1.51120974849783,1.94137526215855,11.5427765500327));
#30250=CARTESIAN_POINT('Ctrl Pts',(1.56743935204678,1.90074932215926,11.5399206494764));
#30251=CARTESIAN_POINT('Ctrl Pts',(1.621783737959,1.85766460010194,11.5370660098083));
#30252=CARTESIAN_POINT('Ctrl Pts',(1.64895593091511,1.83612223907328,11.5356386899743));
#30253=CARTESIAN_POINT('Ctrl Pts',(1.67565661487015,1.81396489287275,11.5342116853624));
#30254=CARTESIAN_POINT('Ctrl Pts',(1.70185926132131,1.79119431574093,11.532784659546));
#30255=CARTESIAN_POINT('Ctrl Pts',(1.71882166156475,1.77645368090452,11.5318608680083));
#30256=CARTESIAN_POINT('Ctrl Pts',(1.73557532962421,1.76145603809249,11.5309370675846));
#30257=CARTESIAN_POINT('Ctrl Pts',(1.75211281381839,1.74620161928424,11.5300131670071));
#30258=CARTESIAN_POINT('Ctrl Pts',(1.76112158754248,1.73789179381609,11.529509873329));
#30259=CARTESIAN_POINT('Ctrl Pts',(1.77006808708219,1.72950393138366,11.5290064421071));
#30260=CARTESIAN_POINT('Ctrl Pts',(1.77894146971999,1.72104732904951,11.5285034067769));
#30261=CARTESIAN_POINT('Ctrl Pts',(1.83933200754334,1.66349331791721,11.5250798449438));
#30262=CARTESIAN_POINT('Ctrl Pts',(1.8963984276916,1.60270624192685,11.5216713230637));
#30263=CARTESIAN_POINT('Ctrl Pts',(1.95011819953022,1.53907807970147,11.5182734051049));
#30264=CARTESIAN_POINT('Ctrl Pts',(2.00542449571231,1.47357076525995,11.5147751352761));
#30265=CARTESIAN_POINT('Ctrl Pts',(2.05718398574646,1.40505149787053,11.511288104956));
#30266=CARTESIAN_POINT('Ctrl Pts',(2.10533946111886,1.3339039115796,11.5078074733588));
#30267=CARTESIAN_POINT('Ctrl Pts',(2.15154257592138,1.26564085173229,11.5044679565119));
#30268=CARTESIAN_POINT('Ctrl Pts',(2.19442802485129,1.19495736996561,11.5011343300606));
#30269=CARTESIAN_POINT('Ctrl Pts',(2.23391281993103,1.12216394079048,11.4978023184486));
#30270=CARTESIAN_POINT('Ctrl Pts',(2.25118741777841,1.09031681552637,11.4963445633684));
#30271=CARTESIAN_POINT('Ctrl Pts',(2.26781067606573,1.05806553560368,11.4948871173785));
#30272=CARTESIAN_POINT('Ctrl Pts',(2.28377353610697,1.02543493097626,11.4934296224428));
#30273=CARTESIAN_POINT('Ctrl Pts',(2.29326703470383,1.00602872191068,11.4925628149854));
#30274=CARTESIAN_POINT('Ctrl Pts',(2.30252692730832,0.986488335264957,11.4916959902159));
#30275=CARTESIAN_POINT('Ctrl Pts',(2.31155107931692,0.966818908506685,11.4908290728209));
#30276=CARTESIAN_POINT('Ctrl Pts',(2.31863529945096,0.951377840034761,11.490148517611));
#30277=CARTESIAN_POINT('Ctrl Pts',(2.32557538886546,0.935854346809815,11.4894677807698));
#30278=CARTESIAN_POINT('Ctrl Pts',(2.33236053374086,0.920273937348818,11.4887878255595));
#30279=CARTESIAN_POINT('Ctrl Pts',(2.36796902716184,0.838507826532316,11.4852194152932));
#30280=CARTESIAN_POINT('Ctrl Pts',(2.39937221583678,0.755052917299449,11.4816670269197));
#30281=CARTESIAN_POINT('Ctrl Pts',(2.42650990964853,0.670313949715511,11.4781256336386));
#30282=CARTESIAN_POINT('Ctrl Pts',(2.45395171326163,0.584625382258507,11.4745445548773));
#30283=CARTESIAN_POINT('Ctrl Pts',(2.47703230477293,0.497622920338958,11.470974719015));
#30284=CARTESIAN_POINT('Ctrl Pts',(2.49564463758615,0.409696684762178,11.4674109283565));
#30285=CARTESIAN_POINT('Ctrl Pts',(2.51256694354607,0.329754279086013,11.464170735066));
#30286=CARTESIAN_POINT('Ctrl Pts',(2.52579526118549,0.24904737731457,11.460935538995));
#30287=CARTESIAN_POINT('Ctrl Pts',(2.53521313973642,0.167858755145902,11.4577014336506));
#30288=CARTESIAN_POINT('Ctrl Pts',(2.53942638325848,0.131537684050459,11.4562546032081));
#30289=CARTESIAN_POINT('Ctrl Pts',(2.54287653840534,0.0951201284473648,
11.4548079910601));
#30290=CARTESIAN_POINT('Ctrl Pts',(2.54555076253572,0.0586312673898904,
11.4533612474409));
#30291=CARTESIAN_POINT('Ctrl Pts',(2.54678080763582,0.0418477284777441,
11.4526957983935));
#30292=CARTESIAN_POINT('Ctrl Pts',(2.54784667039524,0.0250491043820508,
11.4520303215313));
#30293=CARTESIAN_POINT('Ctrl Pts',(2.54874698931854,0.00823785327091157,
11.4513647828174));
#30294=CARTESIAN_POINT('Ctrl Pts',(2.54950258918657,-0.00587112388394168,
11.4508062241208));
#30295=CARTESIAN_POINT('Ctrl Pts',(2.55014158604825,-0.0199907301096276,
11.4502475533557));
#30296=CARTESIAN_POINT('Ctrl Pts',(2.55066270854233,-0.0341027028361791,
11.4496894146469));
#30297=CARTESIAN_POINT('Ctrl Pts',(2.55400035119776,-0.124485909584641,
11.4461146935723));
#30298=CARTESIAN_POINT('Ctrl Pts',(2.55251590030915,-0.214700787372498,
11.4425560101414));
#30299=CARTESIAN_POINT('Ctrl Pts',(2.54610973516166,-0.304360270645855,
11.4390083150826));
#30300=CARTESIAN_POINT('Ctrl Pts',(2.53992350143221,-0.390941635131681,
11.4355824166973));
#30301=CARTESIAN_POINT('Ctrl Pts',(2.52914771427487,-0.477005973362024,
11.4321667651471));
#30302=CARTESIAN_POINT('Ctrl Pts',(2.51364702202946,-0.56221151242787,11.4287568135539));
#30303=CARTESIAN_POINT('Ctrl Pts',(2.4978416408886,-0.649091891634602,11.4252798343488));
#30304=CARTESIAN_POINT('Ctrl Pts',(2.47712400969773,-0.735080204165537,
11.4218087813851));
#30305=CARTESIAN_POINT('Ctrl Pts',(2.45176245019841,-0.819915179815436,
11.4183388343531));
#30306=CARTESIAN_POINT('Ctrl Pts',(2.43759878319083,-0.867292958210081,
11.4164009734618));
#30307=CARTESIAN_POINT('Ctrl Pts',(2.42198578511571,-0.914310849766526,
11.4144634574981));
#30308=CARTESIAN_POINT('Ctrl Pts',(2.40496360252248,-0.960921226687823,
11.4125254468584));
#30309=CARTESIAN_POINT('Ctrl Pts',(2.39839032938233,-0.978920254544038,
11.4117770661373));
#30310=CARTESIAN_POINT('Ctrl Pts',(2.39160484182306,-0.996863365779891,
11.4110284061025));
#30311=CARTESIAN_POINT('Ctrl Pts',(2.38462104532031,-1.01471861919519,11.4102806421704));
#30312=CARTESIAN_POINT('Ctrl Pts',(2.35196925304181,-1.09819843212604,11.4067845734384));
#30313=CARTESIAN_POINT('Ctrl Pts',(2.31495075727319,-1.17986515814379,11.4033036769767));
#30314=CARTESIAN_POINT('Ctrl Pts',(2.27389075093231,-1.25946542646749,11.3998332297369));
#30315=CARTESIAN_POINT('Ctrl Pts',(2.23207387867294,-1.34053297976178,11.3962988111666));
#30316=CARTESIAN_POINT('Ctrl Pts',(2.18606471254661,-1.41945796930655,11.3927752305933));
#30317=CARTESIAN_POINT('Ctrl Pts',(2.13615274225743,-1.49596025824322,11.3892574989426));
#30318=CARTESIAN_POINT('Ctrl Pts',(2.08602408315185,-1.57279467573233,11.385724495342));
#30319=CARTESIAN_POINT('Ctrl Pts',(2.03195810671375,-1.64718611516111,11.3821973915595));
#30320=CARTESIAN_POINT('Ctrl Pts',(1.97420160691916,-1.71882633760539,11.3786711332592));
#30321=CARTESIAN_POINT('Ctrl Pts',(1.95240508667088,-1.74586238661548,11.377340371168));
#30322=CARTESIAN_POINT('Ctrl Pts',(1.93008253152955,-1.77250629512415,11.3760097294909));
#30323=CARTESIAN_POINT('Ctrl Pts',(1.90724574604483,-1.79874022848494,11.3746789365696));
#30324=CARTESIAN_POINT('Ctrl Pts',(1.89585779635524,-1.81182222347379,11.3740153141501));
#30325=CARTESIAN_POINT('Ctrl Pts',(1.8843419621495,-1.82480225835256,11.3733516541209));
#30326=CARTESIAN_POINT('Ctrl Pts',(1.87269964124851,-1.83767804526001,11.3726879227956));
#30327=CARTESIAN_POINT('Ctrl Pts',(1.86326625859819,-1.8481108640987,11.3721501235353));
#30328=CARTESIAN_POINT('Ctrl Pts',(1.8537496389451,-1.8584753407347,11.3716122696922));
#30329=CARTESIAN_POINT('Ctrl Pts',(1.8441608279676,-1.86875948192732,11.3710749125616));
#30330=CARTESIAN_POINT('Ctrl Pts',(1.78056218360928,-1.93696996597738,11.3675108434478));
#30331=CARTESIAN_POINT('Ctrl Pts',(1.71368420494736,-2.00176842633816,11.3639624618779));
#30332=CARTESIAN_POINT('Ctrl Pts',(1.64382533951827,-2.06287172496906,11.3604247664903));
#30333=CARTESIAN_POINT('Ctrl Pts',(1.57423141411002,-2.12374328910052,11.3569004878264));
#30334=CARTESIAN_POINT('Ctrl Pts',(1.50167852811227,-2.18094842953722,11.3533868144436));
#30335=CARTESIAN_POINT('Ctrl Pts',(1.42641996197867,-2.2341772386581,11.3498788016679));
#30336=CARTESIAN_POINT('Ctrl Pts',(1.3516762241841,-2.28704192046701,11.3463947864845));
#30337=CARTESIAN_POINT('Ctrl Pts',(1.27426307539374,-2.33598522008376,11.342916354727));
#30338=CARTESIAN_POINT('Ctrl Pts',(1.19439676647842,-2.38066281826916,11.339438662505));
#30339=CARTESIAN_POINT('Ctrl Pts',(1.15339338620205,-2.40360030684365,11.3376532145659));
#30340=CARTESIAN_POINT('Ctrl Pts',(1.11174294293827,-2.42541271468527,11.3358679615534));
#30341=CARTESIAN_POINT('Ctrl Pts',(1.06947220915485,-2.44604826098259,11.334082247983));
#30342=CARTESIAN_POINT('Ctrl Pts',(1.05124776879456,-2.45494499044852,11.3333123623541));
#30343=CARTESIAN_POINT('Ctrl Pts',(1.0329023157667,-2.46362538871231,11.3325421557385));
#30344=CARTESIAN_POINT('Ctrl Pts',(1.01446903163988,-2.47207123914098,11.3317728670993));
#30345=CARTESIAN_POINT('Ctrl Pts',(0.992379075227472,-2.48219252119531,
11.3308509720972));
#30346=CARTESIAN_POINT('Ctrl Pts',(0.970156538466361,-2.49198036655811,
11.3299301186847));
#30347=CARTESIAN_POINT('Ctrl Pts',(0.94780620569595,-2.50142961190602,11.3290102203308));
#30348=CARTESIAN_POINT('Ctrl Pts',(0.865790439448149,-2.53610413356231,
11.3256346031023));
#30349=CARTESIAN_POINT('Ctrl Pts',(0.78205610317221,-2.56622272676918,11.3222718463403));
#30350=CARTESIAN_POINT('Ctrl Pts',(0.696974578785958,-2.59191739767486,
11.318917674299));
#30351=CARTESIAN_POINT('Ctrl Pts',(0.609579162327931,-2.61831086536073,
11.3154722816062));
#30352=CARTESIAN_POINT('Ctrl Pts',(0.520761565645775,-2.64003666842693,
11.3120359469267));
#30353=CARTESIAN_POINT('Ctrl Pts',(0.430899300361841,-2.65718927641842,
11.3086040360895));
#30354=CARTESIAN_POINT('Ctrl Pts',(0.343209845834361,-2.67392714557567,
11.3052551066101));
#30355=CARTESIAN_POINT('Ctrl Pts',(0.25452479015491,-2.6863100783274,11.3019103896282));
#30356=CARTESIAN_POINT('Ctrl Pts',(0.165183352753207,-2.69438132192965,
11.2985655790638));
#30357=CARTESIAN_POINT('Ctrl Pts',(0.137834848150192,-2.69685202812409,
11.2975416917191));
#30358=CARTESIAN_POINT('Ctrl Pts',(0.110424801620538,-2.69891839950379,
11.2965177956053));
#30359=CARTESIAN_POINT('Ctrl Pts',(0.08296290180991,-2.70058085938097,11.2954937672061));
#30360=CARTESIAN_POINT('Ctrl Pts',(0.0669684788561147,-2.70154911309258,
11.2948973502268));
#30361=CARTESIAN_POINT('Ctrl Pts',(0.0509564666454086,-2.70238034652659,
11.2943008883741));
#30362=CARTESIAN_POINT('Ctrl Pts',(0.0349287839010169,-2.70307458363613,
11.2937043572455));
#30363=CARTESIAN_POINT('Ctrl Pts',(0.0206834334719444,-2.70369161924033,
11.293174162388));
#30364=CARTESIAN_POINT('Ctrl Pts',(0.00643409067270473,-2.70420004997344,
11.2926442249703));
#30365=CARTESIAN_POINT('Ctrl Pts',(-0.00781400179505987,-2.70460019597085,
11.2921146711228));
#30366=CARTESIAN_POINT('Ctrl Pts',(-0.101952151334104,-2.70724398873305,
11.2886158715889));
#30367=CARTESIAN_POINT('Ctrl Pts',(-0.196088226677417,-2.7051673117304,
11.2851318105594));
#30368=CARTESIAN_POINT('Ctrl Pts',(-0.289825667638303,-2.6984813516168,
11.2816577549713));
#30369=CARTESIAN_POINT('Ctrl Pts',(-0.384631538117472,-2.69171918420471,
11.2781441017209));
#30370=CARTESIAN_POINT('Ctrl Pts',(-0.479030586990251,-2.68024208441543,
11.2746406832979));
#30371=CARTESIAN_POINT('Ctrl Pts',(-0.57262152425153,-2.66411259564997,
11.2711426029439));
#30372=CARTESIAN_POINT('Ctrl Pts',(-0.666559717691804,-2.64792326065578,
11.2676315434484));
#30373=CARTESIAN_POINT('Ctrl Pts',(-0.759684799865766,-2.62704692522732,
11.2641258617076));
#30374=CARTESIAN_POINT('Ctrl Pts',(-0.851585181919148,-2.6014943492988,
11.2606206062542));
#30375=CARTESIAN_POINT('Ctrl Pts',(-0.886047825189167,-2.59191213332561,
11.2593061354592));
#30376=CARTESIAN_POINT('Ctrl Pts',(-0.920338108563248,-2.58167179563189,
11.2579917246108));
#30377=CARTESIAN_POINT('Ctrl Pts',(-0.95443366677234,-2.57077201863537,
11.2566771125966));
#30378=CARTESIAN_POINT('Ctrl Pts',(-0.974280480974564,-2.5644273256531,
11.255911885049));
#30379=CARTESIAN_POINT('Ctrl Pts',(-0.99406130744013,-2.55785917358927,
11.2551465893396));
#30380=CARTESIAN_POINT('Ctrl Pts',(-1.01377165408274,-2.55106714297751,
11.2543811739687));
#30381=CARTESIAN_POINT('Ctrl Pts',(-1.02736841414217,-2.54638180627496,
11.2538531685848));
#30382=CARTESIAN_POINT('Ctrl Pts',(-1.04092225787931,-2.54159315279905,
11.253325470206));
#30383=CARTESIAN_POINT('Ctrl Pts',(-1.05443025528497,-2.53670205395909,
11.252798124302));
#30384=CARTESIAN_POINT('Ctrl Pts',(-1.14463510839177,-2.50403985843604,
11.2492765690056));
#30385=CARTESIAN_POINT('Ctrl Pts',(-1.23281912858369,-2.46680540724472,
11.2457698275395));
#30386=CARTESIAN_POINT('Ctrl Pts',(-1.31858159439492,-2.42506535814129,
11.242273074989));
#30387=CARTESIAN_POINT('Ctrl Pts',(-1.40311199337542,-2.38392494816353,
11.2388265569179));
#30388=CARTESIAN_POINT('Ctrl Pts',(-1.48529083212456,-2.33840727081253,
11.2353897428216));
#30389=CARTESIAN_POINT('Ctrl Pts',(-1.56472199239298,-2.28852750879454,
11.2319580127567));
#30390=CARTESIAN_POINT('Ctrl Pts',(-1.58551758994019,-2.27546866069046,
11.2310595633688));
#30391=CARTESIAN_POINT('Ctrl Pts',(-1.60612474663732,-2.26211056997792,
11.230161462454));
#30392=CARTESIAN_POINT('Ctrl Pts',(-1.62653609083598,-2.2484529714829,11.2292636271078));
#30393=CARTESIAN_POINT('Ctrl Pts',(-1.70441968299709,-2.19633965543995,
11.225837755629));
#30394=CARTESIAN_POINT('Ctrl Pts',(-1.77945485532057,-2.13986885585993,
11.222415750716));
#30395=CARTESIAN_POINT('Ctrl Pts',(-1.85149349468849,-2.07939019092048,
11.2189930066095));
#30396=CARTESIAN_POINT('Ctrl Pts',(-1.8748645479439,-2.05976946915896,11.2178825867641));
#30397=CARTESIAN_POINT('Ctrl Pts',(-1.89791995295043,-2.03972659946025,
11.2167720891179));
#30398=CARTESIAN_POINT('Ctrl Pts',(-1.92065386067013,-2.01927267290743,
11.2156613564032));
#30399=CARTESIAN_POINT('Ctrl Pts',(-1.9316413592642,-2.00938710936888,11.2151245294621));
#30400=CARTESIAN_POINT('Ctrl Pts',(-1.94255421950186,-1.99940498570623,
11.2145876221361));
#30401=CARTESIAN_POINT('Ctrl Pts',(-1.95338011991677,-1.98933864610605,
11.2140511999421));
#30402=CARTESIAN_POINT('Ctrl Pts',(-2.02242773931489,-1.92513550744723,
11.2106298978731));
#30403=CARTESIAN_POINT('Ctrl Pts',(-2.08805585991204,-1.85740773886018,
11.2072227031525));
#30404=CARTESIAN_POINT('Ctrl Pts',(-2.15015903930769,-1.7865606665237,11.2038251982962));
#30405=CARTESIAN_POINT('Ctrl Pts',(-2.21349481278046,-1.71430745552261,
11.2003602613952));
#30406=CARTESIAN_POINT('Ctrl Pts',(-2.27316487566809,-1.63880924004706,
11.1969054028151));
#30407=CARTESIAN_POINT('Ctrl Pts',(-2.32902567586957,-1.56045035084564,
11.1934559367882));
#30408=CARTESIAN_POINT('Ctrl Pts',(-2.38527990190259,-1.48153958249049,
11.1899821762823));
#30409=CARTESIAN_POINT('Ctrl Pts',(-2.43767154642151,-1.39972691196139,
11.1865138845562));
#30410=CARTESIAN_POINT('Ctrl Pts',(-2.48601414345046,-1.31537014370798,
11.1830462761383));
#30411=CARTESIAN_POINT('Ctrl Pts',(-2.51324863986033,-1.26784654664574,
11.1810927491288));
#30412=CARTESIAN_POINT('Ctrl Pts',(-2.53919729042327,-1.21951494628862,
11.1791394389872));
#30413=CARTESIAN_POINT('Ctrl Pts',(-2.56382026308967,-1.17043597842562,
11.1771854900701));
#30414=CARTESIAN_POINT('Ctrl Pts',(-2.57043915220293,-1.15724308533024,
11.1766602500274));
#30415=CARTESIAN_POINT('Ctrl Pts',(-2.57696321367054,-1.1439941193146,11.1761348825453));
#30416=CARTESIAN_POINT('Ctrl Pts',(-2.58338840616944,-1.13069688731366,
11.175609633533));
#30417=CARTESIAN_POINT('Ctrl Pts',(-2.62620034331217,-1.04209561027884,
11.172109827464));
#30418=CARTESIAN_POINT('Ctrl Pts',(-2.66450788394824,-0.951602474453648,
11.1686250464566));
#30419=CARTESIAN_POINT('Ctrl Pts',(-2.69817002472794,-0.859613847080416,
11.1651505728457));
#30420=CARTESIAN_POINT('Ctrl Pts',(-2.73183382450822,-0.767620686151626,
11.1616759279993));
#30421=CARTESIAN_POINT('Ctrl Pts',(-2.76085223666098,-0.67413102162785,
11.1582115915653));
#30422=CARTESIAN_POINT('Ctrl Pts',(-2.78504109696179,-0.579512179774996,
11.1547528451809));
#30423=CARTESIAN_POINT('Ctrl Pts',(-2.80867562760501,-0.487061692675289,
11.1513733619645));
#30424=CARTESIAN_POINT('Ctrl Pts',(-2.8276996967141,-0.393532337548253,
11.1479992155222));
#30425=CARTESIAN_POINT('Ctrl Pts',(-2.84189514122644,-0.299251761426908,
11.1446260045022));
#30426=CARTESIAN_POINT('Ctrl Pts',(-2.85324010443846,-0.223902964369238,
11.1419301428196));
#30427=CARTESIAN_POINT('Ctrl Pts',(-2.86150015598816,-0.148073915036915,
11.1392348786069));
#30428=CARTESIAN_POINT('Ctrl Pts',(-2.86653995619031,-0.0719300717664526,
11.1365379651471));
#30429=CARTESIAN_POINT('Ctrl Pts',(-2.86814414143213,-0.0476932320643782,
11.1356795285827));
#30430=CARTESIAN_POINT('Ctrl Pts',(-2.86941988081495,-0.0234547494955555,
11.1348219958471));
#30431=CARTESIAN_POINT('Ctrl Pts',(-2.87036479087719,0.000779773978368722,
11.1339652973708));
#30432=CARTESIAN_POINT('',(0.261199069988913,2.92594434598213,11.058));
#30433=CARTESIAN_POINT('Ctrl Pts',(0.261124777554784,2.92529416030266,11.058));
#30434=CARTESIAN_POINT('Ctrl Pts',(0.163252076286772,2.9214051496811,11.0703793245688));
#30435=CARTESIAN_POINT('Ctrl Pts',(0.0658388360676064,2.91286361031638,
11.0828028087884));
#30436=CARTESIAN_POINT('Ctrl Pts',(-0.0307369711720644,2.89968653111402,
11.0952900032599));
#30437=CARTESIAN_POINT('Ctrl Pts',(-0.12623809978967,2.88665608413482,11.1076382424244));
#30438=CARTESIAN_POINT('Ctrl Pts',(-0.220921197195477,2.86909236615812,
11.1200487818169));
#30439=CARTESIAN_POINT('Ctrl Pts',(-0.31439997383375,2.84696555496448,11.1325405266072));
#30440=CARTESIAN_POINT('Ctrl Pts',(-0.389995520831668,2.82907177783499,
11.1426425017756));
#30441=CARTESIAN_POINT('Ctrl Pts',(-0.464803253647579,2.80819289824412,
11.152797583885));
#30442=CARTESIAN_POINT('Ctrl Pts',(-0.538603048202427,2.78429272567688,
11.1630157713274));
#30443=CARTESIAN_POINT('Ctrl Pts',(-0.593952894118562,2.76636759625145,
11.1706794119091));
#30444=CARTESIAN_POINT('Ctrl Pts',(-0.648735503576454,2.7467426089957,11.1783785492407));
#30445=CARTESIAN_POINT('Ctrl Pts',(-0.702851172581185,2.72539620337798,
11.1861174013937));
#30446=CARTESIAN_POINT('Ctrl Pts',(-0.71873840261759,2.71912934457837,11.1883893667345));
#30447=CARTESIAN_POINT('Ctrl Pts',(-0.734568107078247,2.71271408483162,
11.190664755044));
#30448=CARTESIAN_POINT('Ctrl Pts',(-0.750337652372167,2.70614979460715,
11.1929436730527));
#30449=CARTESIAN_POINT('Ctrl Pts',(-0.763539656096334,2.70065427889159,
11.1948515456945));
#30450=CARTESIAN_POINT('Ctrl Pts',(-0.776691326847496,2.69505769580723,
11.1967607130315));
#30451=CARTESIAN_POINT('Ctrl Pts',(-0.789788993683481,2.68936106997679,
11.1986708957826));
#30452=CARTESIAN_POINT('Ctrl Pts',(-0.87317349082548,2.65309428397392,11.2108318119326));
#30453=CARTESIAN_POINT('Ctrl Pts',(-0.954403883416443,2.61276259333994,
11.2230385405707));
#30454=CARTESIAN_POINT('Ctrl Pts',(-1.03314628688233,2.56834468618871,11.2353100289649));
#30455=CARTESIAN_POINT('Ctrl Pts',(-1.07823214235908,2.54291214597843,11.2423363645588));
#30456=CARTESIAN_POINT('Ctrl Pts',(-1.12250179725942,2.51613922516579,11.2493839310575));
#30457=CARTESIAN_POINT('Ctrl Pts',(-1.16588734321926,2.48801620495338,11.2564562851141));
#30458=CARTESIAN_POINT('Ctrl Pts',(-1.2435976078222,2.43764349916415,11.2691239718505));
#30459=CARTESIAN_POINT('Ctrl Pts',(-1.31847408700313,2.38294042952196,11.2818711829841));
#30460=CARTESIAN_POINT('Ctrl Pts',(-1.39030087935118,2.32423346489716,11.2947183566611));
#30461=CARTESIAN_POINT('Ctrl Pts',(-1.46342993694969,2.26446210581046,11.3077984577361));
#30462=CARTESIAN_POINT('Ctrl Pts',(-1.53339828473794,2.20053932645019,11.3209821789827));
#30463=CARTESIAN_POINT('Ctrl Pts',(-1.59992558939365,2.1327921427514,11.3342910904939));
#30464=CARTESIAN_POINT('Ctrl Pts',(-1.61340208445737,2.11906853570881,11.3369870884937));
#30465=CARTESIAN_POINT('Ctrl Pts',(-1.62674073455187,2.10518403555254,11.3396889690338));
#30466=CARTESIAN_POINT('Ctrl Pts',(-1.63991787601809,2.09116421105248,11.3423925384684));
#30467=CARTESIAN_POINT('Ctrl Pts',(-1.70139884650346,2.02575150993609,11.3550066606613));
#30468=CARTESIAN_POINT('Ctrl Pts',(-1.75944768512028,1.95731714657644,11.3676731670409));
#30469=CARTESIAN_POINT('Ctrl Pts',(-1.8138993651727,1.88618389956551,11.3804137020214));
#30470=CARTESIAN_POINT('Ctrl Pts',(-1.86815753562372,1.81530344486993,11.393108959871));
#30471=CARTESIAN_POINT('Ctrl Pts',(-1.91884436205444,1.74174225535381,11.4058777210929));
#30472=CARTESIAN_POINT('Ctrl Pts',(-1.96574838356875,1.66580180077525,11.4187414001618));
#30473=CARTESIAN_POINT('Ctrl Pts',(-2.01186212788083,1.59114085290088,11.4313883414761));
#30474=CARTESIAN_POINT('Ctrl Pts',(-2.05431959945996,1.51417923664983,11.4441270290762));
#30475=CARTESIAN_POINT('Ctrl Pts',(-2.09287020326133,1.43520021222363,11.4569778131465));
#30476=CARTESIAN_POINT('Ctrl Pts',(-2.11361694660402,1.39269614256837,11.4638937079073));
#30477=CARTESIAN_POINT('Ctrl Pts',(-2.13323129045024,1.34960780406157,11.4708420687169));
#30478=CARTESIAN_POINT('Ctrl Pts',(-2.15166787184208,1.30598030868302,11.4778260675126));
#30479=CARTESIAN_POINT('Ctrl Pts',(-2.15713184571921,1.29305060712901,11.4798958865407));
#30480=CARTESIAN_POINT('Ctrl Pts',(-2.16249308944786,1.28007170317631,11.4819691313049));
#30481=CARTESIAN_POINT('Ctrl Pts',(-2.16774797314523,1.26705068510794,11.4840449452013));
#30482=CARTESIAN_POINT('Ctrl Pts',(-2.19963752356477,1.18803192158837,11.4966421358759));
#30483=CARTESIAN_POINT('Ctrl Pts',(-2.22751419897903,1.10771397257159,11.5092939385505));
#30484=CARTESIAN_POINT('Ctrl Pts',(-2.25120331746379,1.02636717479289,11.5220225137828));
#30485=CARTESIAN_POINT('Ctrl Pts',(-2.27454503464211,0.946213329121761,
11.5345644242532));
#30486=CARTESIAN_POINT('Ctrl Pts',(-2.29382118362004,0.865059764231561,
11.5471808720505));
#30487=CARTESIAN_POINT('Ctrl Pts',(-2.30881496364231,0.783166675687281,
11.5598930570057));
#30488=CARTESIAN_POINT('Ctrl Pts',(-2.3233692591387,0.703673965509062,11.572232633548));
#30489=CARTESIAN_POINT('Ctrl Pts',(-2.33388845327117,0.623483808186223,
11.5846624171728));
#30490=CARTESIAN_POINT('Ctrl Pts',(-2.34012749274977,0.542846284442329,
11.5972017976454));
#30491=CARTESIAN_POINT('Ctrl Pts',(-2.34523853245788,0.476787785015864,
11.6074740954455));
#30492=CARTESIAN_POINT('Ctrl Pts',(-2.34747636127652,0.410429125649976,
11.6178199429796));
#30493=CARTESIAN_POINT('Ctrl Pts',(-2.34668236863853,0.343918483395475,
11.62825));
#30494=CARTESIAN_POINT('',(-2.14415473270599,2.01243073062329,11.058));
#30495=CARTESIAN_POINT('Origin',(0.,0.,11.058));
#30496=CARTESIAN_POINT('Ctrl Pts',(-2.87036479087719,0.000779773978368722,
11.1339652973708));
#30497=CARTESIAN_POINT('Ctrl Pts',(-2.87200285191233,0.0427918449624727,
11.1324801566689));
#30498=CARTESIAN_POINT('Ctrl Pts',(-2.87264678506693,0.0847919926152422,
11.1309975229776));
#30499=CARTESIAN_POINT('Ctrl Pts',(-2.87228289058568,0.126751532711213,
11.1295170338848));
#30500=CARTESIAN_POINT('Ctrl Pts',(-2.87145802595519,0.221864106052536,
11.1261611075067));
#30501=CARTESIAN_POINT('Ctrl Pts',(-2.86545855469524,0.316767622116373,
11.1228162005919));
#30502=CARTESIAN_POINT('Ctrl Pts',(-2.85455763680452,0.411156736693552,
11.1194780920563));
#30503=CARTESIAN_POINT('Ctrl Pts',(-2.84342076253498,0.507588955704657,
11.1160677283208));
#30504=CARTESIAN_POINT('Ctrl Pts',(-2.82716775830471,0.603485022278454,
11.1126644604589));
#30505=CARTESIAN_POINT('Ctrl Pts',(-2.80603441756026,0.698520670355508,
11.1092637873076));
#30506=CARTESIAN_POINT('Ctrl Pts',(-2.79266006313991,0.75866451866233,11.1071116520374));
#30507=CARTESIAN_POINT('Ctrl Pts',(-2.77733000149192,0.818463754777881,
11.1049605559651));
#30508=CARTESIAN_POINT('Ctrl Pts',(-2.76009348614301,0.877834296726592,
11.1028093582138));
#30509=CARTESIAN_POINT('Ctrl Pts',(-2.74919109087412,0.915387195473845,
11.1014486882808));
#30510=CARTESIAN_POINT('Ctrl Pts',(-2.73752580613221,0.952768545576029,
11.1000879776682));
#30511=CARTESIAN_POINT('Ctrl Pts',(-2.72510854264357,0.989956497598032,
11.0987269376699));
#30512=CARTESIAN_POINT('Ctrl Pts',(-2.72027063675402,1.00444534308902,11.0981966611375));
#30513=CARTESIAN_POINT('Ctrl Pts',(-2.71531799003855,1.0189064745382,11.0976662739811));
#30514=CARTESIAN_POINT('Ctrl Pts',(-2.71025302608607,1.03333338889234,11.0971359498549));
#30515=CARTESIAN_POINT('Ctrl Pts',(-2.67741979989202,1.12685471435798,11.0936981658637));
#30516=CARTESIAN_POINT('Ctrl Pts',(-2.63998428261572,1.2186200392303,11.0902747408666));
#30517=CARTESIAN_POINT('Ctrl Pts',(-2.59822193704792,1.30830487286322,11.0868612068006));
#30518=CARTESIAN_POINT('Ctrl Pts',(-2.55598691495593,1.39900478155616,11.0834090375144));
#30519=CARTESIAN_POINT('Ctrl Pts',(-2.50932621498891,1.48757769234242,11.0799669843223));
#30520=CARTESIAN_POINT('Ctrl Pts',(-2.45847158858181,1.57367848927911,11.0765304257261));
#30521=CARTESIAN_POINT('Ctrl Pts',(-2.40788866695146,1.65931926911486,11.0731122278858));
#30522=CARTESIAN_POINT('Ctrl Pts',(-2.35315604081231,1.74251510638125,11.0696994660854));
#30523=CARTESIAN_POINT('Ctrl Pts',(-2.29445585803367,1.82290449738493,11.0662875925062));
#30524=CARTESIAN_POINT('Ctrl Pts',(-2.24693123162509,1.88798906090443,11.0635252839489));
#30525=CARTESIAN_POINT('Ctrl Pts',(-2.19680500482205,1.95123384018432,11.0607635576017));
#30526=CARTESIAN_POINT('Ctrl Pts',(-2.14415473270599,2.01243073062329,11.058));
#30527=CARTESIAN_POINT('',(-2.,-2.4492935982947E-16,12.));
#30528=CARTESIAN_POINT('',(-2.5,-3.06161699786838E-16,11.5));
#30529=CARTESIAN_POINT('Origin',(0.,0.,12.));
#30530=CARTESIAN_POINT('Ctrl Pts',(1.70810875200395,-2.39535560853238,-0.329233991005387));
#30531=CARTESIAN_POINT('Ctrl Pts',(2.49644455514999,-1.833199709811,-0.276854486500882));
#30532=CARTESIAN_POINT('Ctrl Pts',(3.46233357982621,0.120022568706166,-0.172095477491873));
#30533=CARTESIAN_POINT('Ctrl Pts',(1.80423238277522,2.96114098648209,-0.0149569639783592));
#30534=CARTESIAN_POINT('Ctrl Pts',(-1.47579564172449,3.13432118289611,0.142181549535154));
#30535=CARTESIAN_POINT('Ctrl Pts',(-3.42956675747562,0.496557026061836,
0.299320063048668));
#30536=CARTESIAN_POINT('Ctrl Pts',(-2.30343226514234,-2.58935922774548,
0.456458576562181));
#30537=CARTESIAN_POINT('Ctrl Pts',(0.891761112414455,-3.34848577424617,
0.613597090075694));
#30538=CARTESIAN_POINT('Ctrl Pts',(3.2859015926111,-1.1007252807108,0.770735603589207));
#30539=CARTESIAN_POINT('Ctrl Pts',(2.7288317609948,2.13597203247546,0.927874117102722));
#30540=CARTESIAN_POINT('Ctrl Pts',(-0.27919655644097,3.45406211813255,1.08501263061624));
#30541=CARTESIAN_POINT('Ctrl Pts',(-3.03644606033952,1.66993460430069,1.24215114412975));
#30542=CARTESIAN_POINT('Ctrl Pts',(-3.06648780987738,-1.61410638094873,
1.39928965764326));
#30543=CARTESIAN_POINT('Ctrl Pts',(-0.342327145073366,-3.44839767949667,
1.55642817115678));
#30544=CARTESIAN_POINT('Ctrl Pts',(2.68929601578421,-2.18548654390084,1.71356668467029));
#30545=CARTESIAN_POINT('Ctrl Pts',(3.30550092715682,1.04034856780235,1.8707051981838));
#30546=CARTESIAN_POINT('Ctrl Pts',(0.952834920914103,3.33178039838987,2.02784371169731));
#30547=CARTESIAN_POINT('Ctrl Pts',(-2.25562944112346,2.630740466173,2.18498222521083));
#30548=CARTESIAN_POINT('Ctrl Pts',(-3.43817673987435,-0.433127500149091,
2.34212073872434));
#30549=CARTESIAN_POINT('Ctrl Pts',(-1.53268946892128,-3.10797698807607,
2.49925925223786));
#30550=CARTESIAN_POINT('Ctrl Pts',(1.7493988709872,-2.99136460950407,2.65639776575137));
#30551=CARTESIAN_POINT('Ctrl Pts',(3.46024629894863,-0.188026617557356,
2.81353627926488));
#30552=CARTESIAN_POINT('Ctrl Pts',(2.06323722577413,2.78418938435949,2.97067479277839));
#30553=CARTESIAN_POINT('Ctrl Pts',(-1.18688998506621,3.25575653825361,3.12781330629191));
#30554=CARTESIAN_POINT('Ctrl Pts',(-3.3709995165217,0.803131807227777,3.28495181980542));
#30555=CARTESIAN_POINT('Ctrl Pts',(-2.52741049074122,-2.37083416635282,
3.44209033331894));
#30556=CARTESIAN_POINT('Ctrl Pts',(0.586198762341201,-3.41541058398195,
3.59922884683245));
#30557=CARTESIAN_POINT('Ctrl Pts',(3.17330745213002,-1.3924001776803,3.75636736034597));
#30558=CARTESIAN_POINT('Ctrl Pts',(2.91027678633445,1.88120904397026,3.91350587385948));
#30559=CARTESIAN_POINT('Ctrl Pts',(0.0333505152943699,3.46519064195013,
4.07064438737299));
#30560=CARTESIAN_POINT('Ctrl Pts',(-2.87352987075533,1.93687493734171,4.22778290088651));
#30561=CARTESIAN_POINT('Ctrl Pts',(-3.19951927885268,-1.33106529716661,
4.38492141440001));
#30562=CARTESIAN_POINT('Ctrl Pts',(-0.651826904677972,-3.40349528097662,
4.54205992791353));
#30563=CARTESIAN_POINT('Ctrl Pts',(2.48131063733581,-2.41904029776201,4.69919844142705));
#30564=CARTESIAN_POINT('Ctrl Pts',(3.38583301773356,0.738101088738959,4.85633695494055));
#30565=CARTESIAN_POINT('Ctrl Pts',(1.24933397805696,3.23230924456058,5.01347546845408));
#30566=CARTESIAN_POINT('Ctrl Pts',(-2.00926747133911,2.82338496663079,5.17061398196758));
#30567=CARTESIAN_POINT('Ctrl Pts',(-3.46322427730269,-0.12139211787978,
5.3277524954811));
#30568=CARTESIAN_POINT('Ctrl Pts',(-1.80664989208085,-2.95713959911133,
5.48489100899462));
#30569=CARTESIAN_POINT('Ctrl Pts',(1.47258603363221,-3.13690114838409,5.64202952250812));
#30570=CARTESIAN_POINT('Ctrl Pts',(3.4292033754596,-0.499222045701823,5.79916803602164));
#30571=CARTESIAN_POINT('Ctrl Pts',(2.30584575575073,2.58683857089803,5.95630654953515));
#30572=CARTESIAN_POINT('Ctrl Pts',(-0.888531402702859,3.34950300605675,
6.11344506304867));
#30573=CARTESIAN_POINT('Ctrl Pts',(-3.28486476693535,1.10377620199891,6.27058357656218));
#30574=CARTESIAN_POINT('Ctrl Pts',(-2.73086240406331,-2.13331876928079,
6.4277220900757));
#30575=CARTESIAN_POINT('Ctrl Pts',(0.275892655912234,-3.45435112336383,
6.5848606035892));
#30576=CARTESIAN_POINT('Ctrl Pts',(3.03485183459055,-1.67282180255638,6.74199911710273));
#30577=CARTESIAN_POINT('Ctrl Pts',(3.06802702248421,1.6111699572782,6.89913763061623));
#30578=CARTESIAN_POINT('Ctrl Pts',(0.345621576330127,3.44807252913389,7.05627614412975));
#30579=CARTESIAN_POINT('Ctrl Pts',(-2.68720751132516,2.18805261171336,7.21341465764325));
#30580=CARTESIAN_POINT('Ctrl Pts',(-3.30649300260574,-1.03718969811004,
7.37055317115678));
#30581=CARTESIAN_POINT('Ctrl Pts',(-0.956017138014702,-3.33086920560938,
7.52769168467029));
#30582=CARTESIAN_POINT('Ctrl Pts',(2.25311553735071,-2.63289362024357,7.68483019818381));
#30583=CARTESIAN_POINT('Ctrl Pts',(3.43858888024395,0.429842977951538,7.84196871169731));
#30584=CARTESIAN_POINT('Ctrl Pts',(1.53565755714059,3.10651158777771,7.99910722521083));
#30585=CARTESIAN_POINT('Ctrl Pts',(-1.74654067132524,2.99303427005181,8.15624573872433));
#30586=CARTESIAN_POINT('Ctrl Pts',(-3.46006514069016,0.191331803382343,
8.31338425223787));
#30587=CARTESIAN_POINT('Ctrl Pts',(-2.06589572612039,-2.78221724805058,
8.47052276575136));
#30588=CARTESIAN_POINT('Ctrl Pts',(1.183779392948,-3.25688886436581,8.62766127926489));
#30589=CARTESIAN_POINT('Ctrl Pts',(3.37023102179748,-0.806351310370959,
8.7847997927784));
#30590=CARTESIAN_POINT('Ctrl Pts',(2.52967359714463,2.36841856552378,8.94193830629191));
#30591=CARTESIAN_POINT('Ctrl Pts',(-0.582935293544439,3.41596954985013,
9.09907681980542));
#30592=CARTESIAN_POINT('Ctrl Pts',(-3.17197740603666,1.3954296219005,9.25621533331893));
#30593=CARTESIAN_POINT('Ctrl Pts',(-2.91206965945989,-1.87842613074489,
9.41335384683245));
#30594=CARTESIAN_POINT('Ctrl Pts',(-0.0366657672894424,-3.46516125435096,
9.57049236034596));
#30595=CARTESIAN_POINT('Ctrl Pts',(2.8716885037831,-1.93961114588268,9.72763087385947));
#30596=CARTESIAN_POINT('Ctrl Pts',(3.20077001198978,1.32799366090119,9.88476938737299));
#30597=CARTESIAN_POINT('Ctrl Pts',(0.655114493273841,3.40289939669598,10.0419079008865));
#30598=CARTESIAN_POINT('Ctrl Pts',(-2.47906919875826,2.42135526672317,10.1990464144));
#30599=CARTESIAN_POINT('Ctrl Pts',(-3.3864019310671,-0.734763106864168,
10.3561849279135));
#30600=CARTESIAN_POINT('Ctrl Pts',(-1.25267830620767,-3.23131219035953,
10.513323441427));
#30601=CARTESIAN_POINT('Ctrl Pts',(2.00706204302524,-2.82492459714601,10.6704619549406));
#30602=CARTESIAN_POINT('Ctrl Pts',(3.46239353138226,0.117358798249391,10.8276004684541));
#30603=CARTESIAN_POINT('Ctrl Pts',(1.81131357477516,2.9568147670617,10.9847389819676));
#30604=CARTESIAN_POINT('Ctrl Pts',(-1.47339811761136,3.13548357068097,11.1418774954811));
#30605=CARTESIAN_POINT('Ctrl Pts',(-2.77050414434575,1.38461669033425,11.2466365044901));
#30606=CARTESIAN_POINT('Ctrl Pts',(-2.91090525077877,0.426608275808828,
11.2990160089946));
#30607=CARTESIAN_POINT('Ctrl Pts',(1.59774743137964,-2.24059110187414,-0.219489327336925));
#30608=CARTESIAN_POINT('Ctrl Pts',(2.33514866714022,-1.71475623207252,-0.167109822832421));
#30609=CARTESIAN_POINT('Ctrl Pts',(3.23863136773739,0.11226788144075,-0.0623508138234118));
#30610=CARTESIAN_POINT('Ctrl Pts',(1.6876604910601,2.76982094937113,0.0947876996901019));
#30611=CARTESIAN_POINT('Ctrl Pts',(-1.38044412748324,2.93181193130462,0.251926213203615));
#30612=CARTESIAN_POINT('Ctrl Pts',(-3.2079816177237,0.464474356210045,0.409064726717129));
#30613=CARTESIAN_POINT('Ctrl Pts',(-2.15460694798876,-2.42206010021071,
0.566203240230643));
#30614=CARTESIAN_POINT('Ctrl Pts',(0.834144210720117,-3.13213929648004,
0.723341753744155));
#30615=CARTESIAN_POINT('Ctrl Pts',(3.07359869399491,-1.02960715343621,0.880480267257669));
#30616=CARTESIAN_POINT('Ctrl Pts',(2.55252127926951,1.99796636155783,1.03761878077118));
#30617=CARTESIAN_POINT('Ctrl Pts',(-0.261157599233816,3.2308943271893,1.19475729428469));
#30618=CARTESIAN_POINT('Ctrl Pts',(-2.84026054414775,1.56203972461538,1.35189580779821));
#30619=CARTESIAN_POINT('Ctrl Pts',(-2.86836128896387,-1.50981857631063,
1.50903432131172));
#30620=CARTESIAN_POINT('Ctrl Pts',(-0.320209305227662,-3.22559586930712,
1.66617283482524));
#30621=CARTESIAN_POINT('Ctrl Pts',(2.51553994814305,-2.04428172839443,1.82331134833875));
#30622=CARTESIAN_POINT('Ctrl Pts',(3.09193171078347,0.973131394588079,1.98044986185226));
#30623=CARTESIAN_POINT('Ctrl Pts',(0.891272025644291,3.1165132590083,2.13758837536578));
#30624=CARTESIAN_POINT('Ctrl Pts',(-2.10989267602029,2.4607676867899,2.29472688887929));
#30625=CARTESIAN_POINT('Ctrl Pts',(-3.21603530707201,-0.405143027346019,
2.4518654023928));
#30626=CARTESIAN_POINT('Ctrl Pts',(-1.43366203071003,-2.90716984129947,
2.60900391590632));
#30627=CARTESIAN_POINT('Ctrl Pts',(1.63636978576396,-2.79809181678146,2.76614242941983));
#30628=CARTESIAN_POINT('Ctrl Pts',(3.23667894658341,-0.175878172207005,
2.92328094293335));
#30629=CARTESIAN_POINT('Ctrl Pts',(1.92993096835312,2.60430223316632,3.08041945644686));
#30630=CARTESIAN_POINT('Ctrl Pts',(-1.11020473535129,3.04540131890859,3.23755796996037));
#30631=CARTESIAN_POINT('Ctrl Pts',(-3.15319842040834,0.751241266431068,
3.39469648347389));
#30632=CARTESIAN_POINT('Ctrl Pts',(-2.36411388612472,-2.21765399601942,
3.5518349969874));
#30633=CARTESIAN_POINT('Ctrl Pts',(0.548324318173406,-3.19474007803184,
3.70897351050091));
#30634=CARTESIAN_POINT('Ctrl Pts',(2.96827928823051,-1.30243686459143,3.86611202401443));
#30635=CARTESIAN_POINT('Ctrl Pts',(2.72224309752783,1.75966367151117,4.02325053752794));
#30636=CARTESIAN_POINT('Ctrl Pts',(0.0311957304148393,3.24130383438475,
4.18038905104146));
#30637=CARTESIAN_POINT('Ctrl Pts',(-2.68787040907414,1.81173297801481,4.33752756455496));
#30638=CARTESIAN_POINT('Ctrl Pts',(-2.99279756247315,-1.24506484557935,
4.49466607806848));
#30639=CARTESIAN_POINT('Ctrl Pts',(-0.609712210321215,-3.18359462564273,
4.65180459158199));
#30640=CARTESIAN_POINT('Ctrl Pts',(2.32099255542547,-2.26274551758992,4.80894310509551));
#30641=CARTESIAN_POINT('Ctrl Pts',(3.16707352551029,0.69041219843154,4.96608161860902));
#30642=CARTESIAN_POINT('Ctrl Pts',(1.16861420681437,3.02346896054623,5.12322013212254));
#30643=CARTESIAN_POINT('Ctrl Pts',(-1.87944821283798,2.64096537936348,5.28035864563605));
#30644=CARTESIAN_POINT('Ctrl Pts',(-3.23946451703395,-0.113548943710187,
5.43749715914956));
#30645=CARTESIAN_POINT('Ctrl Pts',(-1.68992180450333,-2.76607809260859,
5.59463567266307));
#30646=CARTESIAN_POINT('Ctrl Pts',(1.37744189294803,-2.93422520459686,5.75177418617659));
#30647=CARTESIAN_POINT('Ctrl Pts',(3.20764171390784,-0.466967188284919,
5.9089126996901));
#30648=CARTESIAN_POINT('Ctrl Pts',(2.15686450238375,2.41970230361335,6.06605121320362));
#30649=CARTESIAN_POINT('Ctrl Pts',(-0.831123173336083,3.13309080469669,
6.22318972671712));
#30650=CARTESIAN_POINT('Ctrl Pts',(-3.07262885787747,1.03246095396017,6.38032824023064));
#30651=CARTESIAN_POINT('Ctrl Pts',(-2.55442072199701,-1.99548452634149,
6.53746675374416));
#30652=CARTESIAN_POINT('Ctrl Pts',(0.258067164519323,-3.23116465972251,
6.69460526725767));
#30653=CARTESIAN_POINT('Ctrl Pts',(2.83876932171097,-1.56474038029172,6.85174378077119));
#30654=CARTESIAN_POINT('Ctrl Pts',(2.86980105267096,1.50707187568543,7.00888229428469));
#30655=CARTESIAN_POINT('Ctrl Pts',(0.323290882482136,3.22529172698812,7.1660208077982));
#30656=CARTESIAN_POINT('Ctrl Pts',(-2.51358638246349,2.04668200194341,7.32315932131173));
#30657=CARTESIAN_POINT('Ctrl Pts',(-3.09285968799709,-0.970176620232505,
7.48029783482524));
#30658=CARTESIAN_POINT('Ctrl Pts',(-0.89424863892644,-3.11566093861428,
7.63743634833875));
#30659=CARTESIAN_POINT('Ctrl Pts',(2.10754119617984,-2.46278172505391,7.79457486185227));
#30660=CARTESIAN_POINT('Ctrl Pts',(3.21642081895241,0.402070718924034,7.95171337536577));
#30661=CARTESIAN_POINT('Ctrl Pts',(1.43643835002984,2.90579912086969,8.1088518888793));
#30662=CARTESIAN_POINT('Ctrl Pts',(-1.63369625507517,2.79965360015637,8.2659904023928));
#30663=CARTESIAN_POINT('Ctrl Pts',(-3.23650949300394,0.178969809174445,
8.42312891590632));
#30664=CARTESIAN_POINT('Ctrl Pts',(-1.93241770234741,-2.6024575170625,8.58026742941983));
#30665=CARTESIAN_POINT('Ctrl Pts',(1.10729511934404,-3.04646048515613,8.73740594293334));
#30666=CARTESIAN_POINT('Ctrl Pts',(3.15247957831459,-0.75425275669555,8.89454445644686));
#30667=CARTESIAN_POINT('Ctrl Pts',(2.36623077267467,2.21539446774564,9.05168296996036));
#30668=CARTESIAN_POINT('Ctrl Pts',(-0.54527170288688,3.19526292897974,9.20882148347389));
#30669=CARTESIAN_POINT('Ctrl Pts',(-2.96703517673773,1.30527057568604,9.36595999698739));
#30670=CARTESIAN_POINT('Ctrl Pts',(-2.72392013268591,-1.75706056298405,
9.52309851050092));
#30671=CARTESIAN_POINT('Ctrl Pts',(-0.0342967831746755,-3.24127634552548,
9.68023702401442));
#30672=CARTESIAN_POINT('Ctrl Pts',(2.68614801326846,-1.81429239945851,9.83737553752795));
#30673=CARTESIAN_POINT('Ctrl Pts',(2.99396748543899,1.24219166847781,9.99451405104144));
#30674=CARTESIAN_POINT('Ctrl Pts',(0.612787387020777,3.18303724158995,10.151652564555));
#30675=CARTESIAN_POINT('Ctrl Pts',(-2.31889593673789,2.2649109158452,10.3087910780685));
#30676=CARTESIAN_POINT('Ctrl Pts',(-3.16760568121541,-0.687289884375024,
10.465929591582));
#30677=CARTESIAN_POINT('Ctrl Pts',(-1.17174245711238,-3.02253632625886,
10.6230681050955));
#30678=CARTESIAN_POINT('Ctrl Pts',(1.8773852777822,-2.64240553397781,10.780206618609));
#30679=CARTESIAN_POINT('Ctrl Pts',(3.23868744580887,0.109776217839061,10.9373451321225));
#30680=CARTESIAN_POINT('Ctrl Pts',(1.69428416552798,2.76577424803644,11.0944836456361));
#30681=CARTESIAN_POINT('Ctrl Pts',(-1.37820150798437,2.93289921693286,11.2516221591496));
#30682=CARTESIAN_POINT('Ctrl Pts',(-2.59150119982806,1.29515627025004,11.3563811681586));
#30683=CARTESIAN_POINT('Ctrl Pts',(-2.72283095673203,0.399045011671044,
11.4087606726631));
#30684=CARTESIAN_POINT('Ctrl Pts',(1.48738611075532,-2.08582659521589,-0.109744663668464));
#30685=CARTESIAN_POINT('Ctrl Pts',(2.17385277913045,-1.59631275433404,-0.0573651591639592));
#30686=CARTESIAN_POINT('Ctrl Pts',(3.01492915564857,0.104513194175331,0.0473938498450494));
#30687=CARTESIAN_POINT('Ctrl Pts',(1.57108859934498,2.57850091226017,0.204532363358563));
#30688=CARTESIAN_POINT('Ctrl Pts',(-1.28509261324199,2.72930267971312,0.361670876872076));
#30689=CARTESIAN_POINT('Ctrl Pts',(-2.98639647797178,0.432391686358259,
0.51880939038559));
#30690=CARTESIAN_POINT('Ctrl Pts',(-2.00578163083517,-2.25476097267596,
0.675947903899103));
#30691=CARTESIAN_POINT('Ctrl Pts',(0.776527309025778,-2.9157928187139,0.833086417412617));
#30692=CARTESIAN_POINT('Ctrl Pts',(2.86129579537873,-0.958489026161636,
0.99022493092613));
#30693=CARTESIAN_POINT('Ctrl Pts',(2.37621079754423,1.85996069064019,1.14736344443964));
#30694=CARTESIAN_POINT('Ctrl Pts',(-0.243118642026661,3.00772653624605,
1.30450195795316));
#30695=CARTESIAN_POINT('Ctrl Pts',(-2.64407502795598,1.45414484493007,1.46164047146667));
#30696=CARTESIAN_POINT('Ctrl Pts',(-2.67023476805036,-1.40553077167252,
1.61877898498018));
#30697=CARTESIAN_POINT('Ctrl Pts',(-0.298091465381954,-3.00279405911757,
1.7759174984937));
#30698=CARTESIAN_POINT('Ctrl Pts',(2.34178388050189,-1.90307691288803,1.93305601200721));
#30699=CARTESIAN_POINT('Ctrl Pts',(2.87836249441012,0.905914221373807,2.09019452552073));
#30700=CARTESIAN_POINT('Ctrl Pts',(0.829709130374474,2.90124611962672,2.24733303903424));
#30701=CARTESIAN_POINT('Ctrl Pts',(-1.96415591091712,2.2907949074068,2.40447155254775));
#30702=CARTESIAN_POINT('Ctrl Pts',(-2.99389387426969,-0.37715855454295,
2.56161006606126));
#30703=CARTESIAN_POINT('Ctrl Pts',(-1.33463459249878,-2.70636269452286,
2.71874857957478));
#30704=CARTESIAN_POINT('Ctrl Pts',(1.52334070054072,-2.60481902405885,2.87588709308829));
#30705=CARTESIAN_POINT('Ctrl Pts',(3.01311159421818,-0.163729726856653,
3.03302560660181));
#30706=CARTESIAN_POINT('Ctrl Pts',(1.79662471093212,2.42441508197314,3.19016412011532));
#30707=CARTESIAN_POINT('Ctrl Pts',(-1.03351948563637,2.83504609956357,3.34730263362884));
#30708=CARTESIAN_POINT('Ctrl Pts',(-2.93539732429499,0.699350725634357,
3.50444114714234));
#30709=CARTESIAN_POINT('Ctrl Pts',(-2.20081728150821,-2.06447382568602,
3.66157966065586));
#30710=CARTESIAN_POINT('Ctrl Pts',(0.510449874005612,-2.97406957208172,
3.81871817416937));
#30711=CARTESIAN_POINT('Ctrl Pts',(2.763251124331,-1.21247355150257,3.97585668768289));
#30712=CARTESIAN_POINT('Ctrl Pts',(2.5342094087212,1.63811829905208,4.1329952011964));
#30713=CARTESIAN_POINT('Ctrl Pts',(0.029040945535309,3.01741702681936,4.29013371470992));
#30714=CARTESIAN_POINT('Ctrl Pts',(-2.50221094739296,1.68659101868791,4.44727222822342));
#30715=CARTESIAN_POINT('Ctrl Pts',(-2.78607584609361,-1.1590643939921,4.60441074173694));
#30716=CARTESIAN_POINT('Ctrl Pts',(-0.56759751596446,-2.96369397030884,
4.76154925525046));
#30717=CARTESIAN_POINT('Ctrl Pts',(2.16067447351513,-2.10645073741783,4.91868776876396));
#30718=CARTESIAN_POINT('Ctrl Pts',(2.94831403328702,0.642723308124124,5.07582628227749));
#30719=CARTESIAN_POINT('Ctrl Pts',(1.08789443557179,2.81462867653188,5.23296479579099));
#30720=CARTESIAN_POINT('Ctrl Pts',(-1.74962895433684,2.45854579209617,5.39010330930451));
#30721=CARTESIAN_POINT('Ctrl Pts',(-3.01570475676522,-0.105705769540595,
5.54724182281802));
#30722=CARTESIAN_POINT('Ctrl Pts',(-1.57319371692581,-2.57501658610585,
5.70438033633154));
#30723=CARTESIAN_POINT('Ctrl Pts',(1.28229775226384,-2.73154926080963,5.86151884984505));
#30724=CARTESIAN_POINT('Ctrl Pts',(2.98608005235609,-0.434712330868017,
6.01865736335856));
#30725=CARTESIAN_POINT('Ctrl Pts',(2.00788324901678,2.25256603632868,6.17579587687208));
#30726=CARTESIAN_POINT('Ctrl Pts',(-0.773714943969305,2.91667860333663,
6.33293439038559));
#30727=CARTESIAN_POINT('Ctrl Pts',(-2.86039294881959,0.961145705921419,
6.4900729038991));
#30728=CARTESIAN_POINT('Ctrl Pts',(-2.37797903993071,-1.85765028340219,
6.64721141741262));
#30729=CARTESIAN_POINT('Ctrl Pts',(0.240241673126412,-3.0079781960812,6.80434993092612));
#30730=CARTESIAN_POINT('Ctrl Pts',(2.64268680883139,-1.45665895802706,6.96148844443965));
#30731=CARTESIAN_POINT('Ctrl Pts',(2.67157508285772,1.40297379409266,7.11862695795316));
#30732=CARTESIAN_POINT('Ctrl Pts',(0.300960188634146,3.00251092484234,7.27576547146667));
#30733=CARTESIAN_POINT('Ctrl Pts',(-2.33996525360183,1.90531139217345,7.43290398498018));
#30734=CARTESIAN_POINT('Ctrl Pts',(-2.87922637338843,-0.903163542354968,
7.5900424984937));
#30735=CARTESIAN_POINT('Ctrl Pts',(-0.832480139838179,-2.90045267161919,
7.74718101200721));
#30736=CARTESIAN_POINT('Ctrl Pts',(1.96196685500896,-2.29266982986425,7.90431952552073));
#30737=CARTESIAN_POINT('Ctrl Pts',(2.99425275766087,0.37429845989653,8.06145803903424));
#30738=CARTESIAN_POINT('Ctrl Pts',(1.33721914291908,2.70508665396167,8.21859655254775));
#30739=CARTESIAN_POINT('Ctrl Pts',(-1.5208518388251,2.60627293026094,8.37573506606126));
#30740=CARTESIAN_POINT('Ctrl Pts',(-3.01295384531772,0.166607814966547,
8.53287357957478));
#30741=CARTESIAN_POINT('Ctrl Pts',(-1.79893967857444,-2.42269778607442,
8.69001209308829));
#30742=CARTESIAN_POINT('Ctrl Pts',(1.03081084574009,-2.83603210594645,8.8471506066018));
#30743=CARTESIAN_POINT('Ctrl Pts',(2.9347281348317,-0.702154203020143,9.00428912011532));
#30744=CARTESIAN_POINT('Ctrl Pts',(2.20278794820472,2.06237036996751,9.16142763362883));
#30745=CARTESIAN_POINT('Ctrl Pts',(-0.507608112229325,2.97455630810935,
9.31856614714235));
#30746=CARTESIAN_POINT('Ctrl Pts',(-2.7620929474388,1.21511152947157,9.47570466065586));
#30747=CARTESIAN_POINT('Ctrl Pts',(-2.53577060591194,-1.63569499522321,
9.63284317416937));
#30748=CARTESIAN_POINT('Ctrl Pts',(-0.0319277990599106,-3.0173914367,9.78998168768289));
#30749=CARTESIAN_POINT('Ctrl Pts',(2.50060752275382,-1.68897365303435,9.94712020119639));
#30750=CARTESIAN_POINT('Ctrl Pts',(2.78716495888821,1.15638967605443,10.1042587147099));
#30751=CARTESIAN_POINT('Ctrl Pts',(0.570460280767717,2.96317508648391,10.2613972282234));
#30752=CARTESIAN_POINT('Ctrl Pts',(-2.15872267471752,2.10846656496723,10.4185357417369));
#30753=CARTESIAN_POINT('Ctrl Pts',(-2.94880943136371,-0.639816661885883,
10.5756742552505));
#30754=CARTESIAN_POINT('Ctrl Pts',(-1.09080660801709,-2.8137604621582,10.732812768764));
#30755=CARTESIAN_POINT('Ctrl Pts',(1.74770851253917,-2.4598864708096,10.8899512822775));
#30756=CARTESIAN_POINT('Ctrl Pts',(3.01498136023548,0.102193637428725,11.047089795791));
#30757=CARTESIAN_POINT('Ctrl Pts',(1.57725475628079,2.57473372901119,11.2042283093045));
#30758=CARTESIAN_POINT('Ctrl Pts',(-1.28300489835739,2.73031486318474,11.361366822818));
#30759=CARTESIAN_POINT('Ctrl Pts',(-2.41249825531037,1.20569585016584,11.466125831827));
#30760=CARTESIAN_POINT('Ctrl Pts',(-2.53475666268528,0.371481747533259,
11.5185053363315));
#30761=CARTESIAN_POINT('Ctrl Pts',(1.37702479013101,-1.93106208855765,-2.4980018054066E-15));
#30762=CARTESIAN_POINT('Ctrl Pts',(2.01255689112068,-1.47786927659557,0.052379504504502));
#30763=CARTESIAN_POINT('Ctrl Pts',(2.79122694355976,0.0967585069099138,
0.157138513513511));
#30764=CARTESIAN_POINT('Ctrl Pts',(1.45451670762985,2.3871808751492,0.314277027027025));
#30765=CARTESIAN_POINT('Ctrl Pts',(-1.18974109900074,2.52679342812162,0.471415540540538));
#30766=CARTESIAN_POINT('Ctrl Pts',(-2.76481133821986,0.40030901650647,0.628554054054051));
#30767=CARTESIAN_POINT('Ctrl Pts',(-1.85695631368159,-2.0874618451412,0.785692567567565));
#30768=CARTESIAN_POINT('Ctrl Pts',(0.718910407331439,-2.69944634094777,
0.942831081081078));
#30769=CARTESIAN_POINT('Ctrl Pts',(2.64899289676255,-0.887370898887054,
1.09996959459459));
#30770=CARTESIAN_POINT('Ctrl Pts',(2.19990031581894,1.72195501972256,1.25710810810811));
#30771=CARTESIAN_POINT('Ctrl Pts',(-0.225079684819506,2.78455874530281,
1.41424662162162));
#30772=CARTESIAN_POINT('Ctrl Pts',(-2.44788951176421,1.34624996524475,1.57138513513514));
#30773=CARTESIAN_POINT('Ctrl Pts',(-2.47210824713685,-1.30124296703442,
1.72852364864864));
#30774=CARTESIAN_POINT('Ctrl Pts',(-0.275973625536248,-2.77999224892802,
1.88566216216216));
#30775=CARTESIAN_POINT('Ctrl Pts',(2.16802781286073,-1.76187209738162,2.04280067567567));
#30776=CARTESIAN_POINT('Ctrl Pts',(2.66479327803676,0.838697048159531,2.19993918918919));
#30777=CARTESIAN_POINT('Ctrl Pts',(0.76814623510466,2.68597898024514,2.3570777027027));
#30778=CARTESIAN_POINT('Ctrl Pts',(-1.81841914581395,2.1208221280237,2.51421621621621));
#30779=CARTESIAN_POINT('Ctrl Pts',(-2.77175244146736,-0.349174081739879,
2.67135472972972));
#30780=CARTESIAN_POINT('Ctrl Pts',(-1.23560715428754,-2.50555554774625,
2.82849324324324));
#30781=CARTESIAN_POINT('Ctrl Pts',(1.41031161531747,-2.41154623133624,2.98563175675675));
#30782=CARTESIAN_POINT('Ctrl Pts',(2.78954424185296,-0.151581281506301,
3.14277027027027));
#30783=CARTESIAN_POINT('Ctrl Pts',(1.66331845351111,2.24452793077997,3.29990878378378));
#30784=CARTESIAN_POINT('Ctrl Pts',(-0.956834235921451,2.62469088021855,
3.45704729729729));
#30785=CARTESIAN_POINT('Ctrl Pts',(-2.71759622818163,0.647460184837647,
3.61418581081081));
#30786=CARTESIAN_POINT('Ctrl Pts',(-2.03752067689171,-1.91129365535261,
3.77132432432432));
#30787=CARTESIAN_POINT('Ctrl Pts',(0.47257542983782,-2.75339906613161,3.92846283783783));
#30788=CARTESIAN_POINT('Ctrl Pts',(2.55822296043148,-1.12251023841371,4.08560135135135));
#30789=CARTESIAN_POINT('Ctrl Pts',(2.34617571991457,1.51657292659299,4.24273986486486));
#30790=CARTESIAN_POINT('Ctrl Pts',(0.0268861606557786,2.79353021925399,
4.39987837837838));
#30791=CARTESIAN_POINT('Ctrl Pts',(-2.31655148571177,1.56144905936101,4.55701689189189));
#30792=CARTESIAN_POINT('Ctrl Pts',(-2.57935412971408,-1.07306394240484,
4.7141554054054));
#30793=CARTESIAN_POINT('Ctrl Pts',(-0.525482821607704,-2.74379331497496,
4.87129391891892));
#30794=CARTESIAN_POINT('Ctrl Pts',(2.00035639160479,-1.95015595724574,5.02843243243243));
#30795=CARTESIAN_POINT('Ctrl Pts',(2.72955454106374,0.595034417816705,5.18557094594594));
#30796=CARTESIAN_POINT('Ctrl Pts',(1.0071746643292,2.60578839251754,5.34270945945947));
#30797=CARTESIAN_POINT('Ctrl Pts',(-1.61980969583571,2.27612620482886,5.49984797297296));
#30798=CARTESIAN_POINT('Ctrl Pts',(-2.79194499649648,-0.0978625953710016,
5.6569864864865));
#30799=CARTESIAN_POINT('Ctrl Pts',(-1.45646562934828,-2.38395507960311,
5.81412499999999));
#30800=CARTESIAN_POINT('Ctrl Pts',(1.18715361157964,-2.5288733170224,5.97126351351352));
#30801=CARTESIAN_POINT('Ctrl Pts',(2.76451839080433,-0.402457473451116,
6.12840202702702));
#30802=CARTESIAN_POINT('Ctrl Pts',(1.8589019956498,2.08542976904401,6.28554054054054));
#30803=CARTESIAN_POINT('Ctrl Pts',(-0.716306714602523,2.70026640197657,
6.44267905405405));
#30804=CARTESIAN_POINT('Ctrl Pts',(-2.64815703976171,0.889830457882673,
6.59981756756756));
#30805=CARTESIAN_POINT('Ctrl Pts',(-2.20153735786441,-1.71981604046289,
6.75695608108108));
#30806=CARTESIAN_POINT('Ctrl Pts',(0.222416181733502,-2.78479173243988,
6.91409459459459));
#30807=CARTESIAN_POINT('Ctrl Pts',(2.4466042959518,-1.34857753576241,7.0712331081081));
#30808=CARTESIAN_POINT('Ctrl Pts',(2.47334911304448,1.29887571249989,7.22837162162162));
#30809=CARTESIAN_POINT('Ctrl Pts',(0.278629494786153,2.77973012269657,7.38551013513513));
#30810=CARTESIAN_POINT('Ctrl Pts',(-2.16634412474015,1.76394078240349,7.54264864864865));
#30811=CARTESIAN_POINT('Ctrl Pts',(-2.66559305877978,-0.83615046447743,
7.69978716216215));
#30812=CARTESIAN_POINT('Ctrl Pts',(-0.770711640749916,-2.68524440462409,
7.85692567567567));
#30813=CARTESIAN_POINT('Ctrl Pts',(1.81639251383808,-2.12255793467458,8.01406418918919));
#30814=CARTESIAN_POINT('Ctrl Pts',(2.77208469636934,0.346526200869026,8.1712027027027));
#30815=CARTESIAN_POINT('Ctrl Pts',(1.23799993580832,2.50437418705365,8.32834121621622));
#30816=CARTESIAN_POINT('Ctrl Pts',(-1.40800742257503,2.4128922603655,8.48547972972973));
#30817=CARTESIAN_POINT('Ctrl Pts',(-2.78939819763151,0.154245820758651,
8.64261824324324));
#30818=CARTESIAN_POINT('Ctrl Pts',(-1.66546165480147,-2.24293805508635,
8.79975675675676));
#30819=CARTESIAN_POINT('Ctrl Pts',(0.954326572136137,-2.62560372673677,
8.95689527027026));
#30820=CARTESIAN_POINT('Ctrl Pts',(2.71697669134881,-0.650055649344734,
9.11403378378378));
#30821=CARTESIAN_POINT('Ctrl Pts',(2.03934512373477,1.90934627218937,9.2711722972973));
#30822=CARTESIAN_POINT('Ctrl Pts',(-0.469944521571767,2.75384968723896,
9.42831081081079));
#30823=CARTESIAN_POINT('Ctrl Pts',(-2.55715071813987,1.12495248325711,9.58544932432433));
#30824=CARTESIAN_POINT('Ctrl Pts',(-2.34762107913798,-1.51432942746238,
9.74258783783783));
#30825=CARTESIAN_POINT('Ctrl Pts',(-0.0295588149451427,-2.79350652787453,
9.89972635135136));
#30826=CARTESIAN_POINT('Ctrl Pts',(2.31506703223917,-1.56365490661018,10.0568648648649));
#30827=CARTESIAN_POINT('Ctrl Pts',(2.58036243233743,1.07058768363104,10.2140033783784));
#30828=CARTESIAN_POINT('Ctrl Pts',(0.528133174514654,2.74331293137788,10.3711418918919));
#30829=CARTESIAN_POINT('Ctrl Pts',(-1.99854941269714,1.95202221408926,10.5282804054054));
#30830=CARTESIAN_POINT('Ctrl Pts',(-2.73001318151202,-0.59234343939674,
10.6854189189189));
#30831=CARTESIAN_POINT('Ctrl Pts',(-1.0098707589218,-2.60498459805753,10.8425574324324));
#30832=CARTESIAN_POINT('Ctrl Pts',(1.61803174729613,-2.2773674076414,10.999695945946));
#30833=CARTESIAN_POINT('Ctrl Pts',(2.79127527466209,0.0946110570183949,
11.1568344594594));
#30834=CARTESIAN_POINT('Ctrl Pts',(1.46022534703361,2.38369320998594,11.313972972973));
#30835=CARTESIAN_POINT('Ctrl Pts',(-1.1878082887304,2.52773050943662,11.4711114864865));
#30836=CARTESIAN_POINT('Ctrl Pts',(-2.23349531079268,1.11623543008163,11.5758704954955));
#30837=CARTESIAN_POINT('Ctrl Pts',(-2.34668236863853,0.343918483395475,
11.62825));
#30838=CARTESIAN_POINT('',(1.37702479013102,-1.93106208855765,0.));
#30839=CARTESIAN_POINT('Ctrl Pts',(1.37702479013101,-1.93106208855765,-2.4980018054066E-15));
#30840=CARTESIAN_POINT('Ctrl Pts',(2.01255689112068,-1.47786927659557,0.052379504504502));
#30841=CARTESIAN_POINT('Ctrl Pts',(2.79122694355976,0.0967585069099138,
0.157138513513511));
#30842=CARTESIAN_POINT('Ctrl Pts',(1.45451670762985,2.3871808751492,0.314277027027025));
#30843=CARTESIAN_POINT('Ctrl Pts',(-1.18974109900074,2.52679342812162,0.471415540540538));
#30844=CARTESIAN_POINT('Ctrl Pts',(-2.31615344009055,1.00603694073732,0.583793234229858));
#30845=CARTESIAN_POINT('Ctrl Pts',(-2.37458477423974,0.11510370689526,0.643791423414673));
#30846=CARTESIAN_POINT('Ctrl Pts',(-2.37366757034868,0.001844716469488,
0.651410108094984));
#30847=CARTESIAN_POINT('Ctrl Pts',(1.29197400994444,2.64783394680711,-2.46330733588707E-16));
#30848=CARTESIAN_POINT('Ctrl Pts',(1.37074936016223,2.60046826619745,-2.90204607120186E-16));
#30849=CARTESIAN_POINT('Ctrl Pts',(1.44700091320012,2.54930204226795,-5.92854700626308E-16));
#30850=CARTESIAN_POINT('Ctrl Pts',(1.5204041597113,2.49432533414619,-4.68375338513738E-16));
#30851=CARTESIAN_POINT('Ctrl Pts',(1.59876972116939,2.43563200920691,-3.1748808003354E-16));
#30852=CARTESIAN_POINT('Ctrl Pts',(1.67388955782072,2.37259497158855,9.42702435984343E-17));
#30853=CARTESIAN_POINT('Ctrl Pts',(1.74558455766593,2.30559334150577,2.91433543964104E-16));
#30854=CARTESIAN_POINT('Ctrl Pts',(1.78514524738377,2.26862241321206,4.00226572297347E-16));
#30855=CARTESIAN_POINT('Ctrl Pts',(1.82366240526687,2.23044382157621,2.41712413072573E-16));
#30856=CARTESIAN_POINT('Ctrl Pts',(1.86109995619813,2.19111823230724,2.56739074444567E-16));
#30857=CARTESIAN_POINT('Ctrl Pts',(1.87813922122651,2.17321964863167,2.63578284255041E-16));
#30858=CARTESIAN_POINT('Ctrl Pts',(1.89495840460327,2.15507923207588,-5.32738877742354E-17));
#30859=CARTESIAN_POINT('Ctrl Pts',(1.91153266312519,2.13672660521873,-9.0205620750794E-17));
#30860=CARTESIAN_POINT('Ctrl Pts',(1.97664662778045,2.0646261070319,-2.35296368099375E-16));
#30861=CARTESIAN_POINT('Ctrl Pts',(2.03804038590891,1.98919650283574,-3.72373475267393E-16));
#30862=CARTESIAN_POINT('Ctrl Pts',(2.09554796148623,1.91081666271006,-8.32667268468867E-17));
#30863=CARTESIAN_POINT('Ctrl Pts',(2.14343533270609,1.8455486617107,1.57476549926517E-16));
#30864=CARTESIAN_POINT('Ctrl Pts',(2.18862729734747,1.77823406218829,2.53857300975798E-16));
#30865=CARTESIAN_POINT('Ctrl Pts',(2.23100237945407,1.70908145885149,3.19189119579733E-16));
#30866=CARTESIAN_POINT('Ctrl Pts',(2.2495414778757,1.67882719489164,3.47771790218954E-16));
#30867=CARTESIAN_POINT('Ctrl Pts',(2.26754109313608,1.64822104628506,2.94521883274651E-16));
#30868=CARTESIAN_POINT('Ctrl Pts',(2.28498954152194,1.61728023964544,3.19189119579733E-16));
#30869=CARTESIAN_POINT('Ctrl Pts',(2.29543189661598,1.59876312668031,3.33951695310829E-16));
#30870=CARTESIAN_POINT('Ctrl Pts',(2.30567682494647,1.58012614919259,-6.61366324171955E-18));
#30871=CARTESIAN_POINT('Ctrl Pts',(2.31572165746038,1.56137299470242,-1.38777878078145E-17));
#30872=CARTESIAN_POINT('Ctrl Pts',(2.32292320728395,1.54792809393149,-1.90857347710862E-17));
#30873=CARTESIAN_POINT('Ctrl Pts',(2.33002152872364,1.53442403232929,-1.12870283643031E-16));
#30874=CARTESIAN_POINT('Ctrl Pts',(2.33700969851763,1.52087413145422,-1.11022302462516E-16));
#30875=CARTESIAN_POINT('Ctrl Pts',(2.38058260792534,1.43638725996736,-9.94996979838631E-17));
#30876=CARTESIAN_POINT('Ctrl Pts',(2.41994184512486,1.3499998824768,-3.77842799305168E-16));
#30877=CARTESIAN_POINT('Ctrl Pts',(2.45492973401008,1.26206183108408,-3.7470027081099E-16));
#30878=CARTESIAN_POINT('Ctrl Pts',(2.48961375478266,1.17488751738912,-3.71585035023886E-16));
#30879=CARTESIAN_POINT('Ctrl Pts',(2.52000223755862,1.08618841594484,-4.13121512185277E-16));
#30880=CARTESIAN_POINT('Ctrl Pts',(2.54589150534161,0.996296170221892,-3.7470027081099E-16));
#30881=CARTESIAN_POINT('Ctrl Pts',(2.57095558696702,0.909269120898709,-3.37503655671981E-16));
#30882=CARTESIAN_POINT('Ctrl Pts',(2.59180267862827,0.821123009321661,-1.98135956264892E-16));
#30883=CARTESIAN_POINT('Ctrl Pts',(2.60819974692058,0.732162501184589,-2.77555756156289E-16));
#30884=CARTESIAN_POINT('Ctrl Pts',(2.61796168819389,0.679200152025794,-3.24838075693952E-16));
#30885=CARTESIAN_POINT('Ctrl Pts',(2.62614545111416,0.625949276096869,-2.51374357035676E-17));
#30886=CARTESIAN_POINT('Ctrl Pts',(2.63269335080009,0.572476447093945,0.));
#30887=CARTESIAN_POINT('Ctrl Pts',(2.6352683765624,0.5514477327168,9.88554309620052E-18));
#30888=CARTESIAN_POINT('Ctrl Pts',(2.63759088070415,0.530377846603737,-5.43523939458827E-17));
#30889=CARTESIAN_POINT('Ctrl Pts',(2.63965388200594,0.50930758122065,-2.77555756156289E-17));
#30890=CARTESIAN_POINT('Ctrl Pts',(2.64834931960739,0.420497565576959,8.43485582923526E-17));
#30891=CARTESIAN_POINT('Ctrl Pts',(2.65245297898025,0.3315870178655,7.13394232030532E-17));
#30892=CARTESIAN_POINT('Ctrl Pts',(2.65178792227632,0.242870082265014,1.11022302462516E-16));
#30893=CARTESIAN_POINT('Ctrl Pts',(2.65141677862428,0.193360428001277,1.33167855834344E-16));
#30894=CARTESIAN_POINT('Ctrl Pts',(2.64955959473733,0.143911103160085,2.55410202784461E-16));
#30895=CARTESIAN_POINT('Ctrl Pts',(2.64617859082989,0.0945743399740305,
2.77555756156289E-16));
#30896=CARTESIAN_POINT('Ctrl Pts',(2.63998980161557,0.00426541509996067,
2.91350122435194E-16));
#30897=CARTESIAN_POINT('Ctrl Pts',(2.62869784498548,-0.0856678806083358,
1.22336690906674E-16));
#30898=CARTESIAN_POINT('Ctrl Pts',(2.61249699286393,-0.174890907412304,
1.94289029309402E-16));
#30899=CARTESIAN_POINT('Ctrl Pts',(2.59606370990205,-0.265394001643718,
2.67273655542046E-16));
#30900=CARTESIAN_POINT('Ctrl Pts',(2.57457910556097,-0.355167245076682,
-8.63540186836622E-17));
#30901=CARTESIAN_POINT('Ctrl Pts',(2.54820206281091,-0.443829678011398,
-1.94289029309402E-16));
#30902=CARTESIAN_POINT('Ctrl Pts',(2.5433159398537,-0.460253640057088,-2.14283072550056E-16));
#30903=CARTESIAN_POINT('Ctrl Pts',(2.53826078384047,-0.476642310793062,
2.54370247567095E-16));
#30904=CARTESIAN_POINT('Ctrl Pts',(2.53304532831965,-0.49296952041645,2.4980018054066E-16));
#30905=CARTESIAN_POINT('Ctrl Pts',(2.5060606614482,-0.577446189974434,2.26154741365496E-16));
#30906=CARTESIAN_POINT('Ctrl Pts',(2.47475215402615,-0.660408357948197,
3.47506847049484E-16));
#30907=CARTESIAN_POINT('Ctrl Pts',(2.43933604293942,-0.741555503604727,
2.77555756156289E-16));
#30908=CARTESIAN_POINT('Ctrl Pts',(2.40393876465244,-0.822659498618874,
2.07641862313994E-16));
#30909=CARTESIAN_POINT('Ctrl Pts',(2.3644375894048,-0.901951185787608,-1.23823437954767E-16));
#30910=CARTESIAN_POINT('Ctrl Pts',(2.32100582430644,-0.979100944080977,
-1.11022302462516E-16));
#30911=CARTESIAN_POINT('Ctrl Pts',(2.27823644108386,-1.05507408425856,-9.84163982743666E-17));
#30912=CARTESIAN_POINT('Ctrl Pts',(2.23165476456022,-1.1289707546069,2.53313632717541E-16));
#30913=CARTESIAN_POINT('Ctrl Pts',(2.18139506127574,-1.20043719637909,2.77555756156289E-16));
#30914=CARTESIAN_POINT('Ctrl Pts',(2.16608689289344,-1.2222045418435,2.84939454890925E-16));
#30915=CARTESIAN_POINT('Ctrl Pts',(2.15043733121093,-1.24374612322857,4.37114965090439E-17));
#30916=CARTESIAN_POINT('Ctrl Pts',(2.13444972694369,-1.26505107698559,0.));
#30917=CARTESIAN_POINT('Ctrl Pts',(2.12083931058568,-1.28318820912085,-3.72120586158607E-17));
#30918=CARTESIAN_POINT('Ctrl Pts',(2.10698390104784,-1.30115384375424,6.4814165885223E-17));
#30919=CARTESIAN_POINT('Ctrl Pts',(2.09288546869145,-1.31894102140198,5.55111512312578E-17));
#30920=CARTESIAN_POINT('Ctrl Pts',(2.08472665052523,-1.32923453095322,5.01274601200272E-17));
#30921=CARTESIAN_POINT('Ctrl Pts',(2.07648733901943,-1.33946704131009,1.07093663002969E-16));
#30922=CARTESIAN_POINT('Ctrl Pts',(2.06817568052718,-1.3496280615777,1.11022302462516E-16));
#30923=CARTESIAN_POINT('Ctrl Pts',(2.0141423836499,-1.41568388247163,1.36562011828508E-16));
#30924=CARTESIAN_POINT('Ctrl Pts',(1.95696807639868,-1.47883106712894,-2.06909962337776E-16));
#30925=CARTESIAN_POINT('Ctrl Pts',(1.89681447147471,-1.5387754276769,-2.22044604925031E-16));
#30926=CARTESIAN_POINT('Ctrl Pts',(1.83758356202805,-1.5978003023447,-2.36947097397864E-16));
#30927=CARTESIAN_POINT('Ctrl Pts',(1.77546340770889,-1.65372037608364,4.0590157288843E-16));
#30928=CARTESIAN_POINT('Ctrl Pts',(1.71058212140457,-1.70621256947127,4.44089209850063E-16));
#30929=CARTESIAN_POINT('Ctrl Pts',(1.64772546517897,-1.75706673624623,4.81085195985522E-16));
#30930=CARTESIAN_POINT('Ctrl Pts',(1.58227673616169,-1.80470390837557,2.58606592525932E-16));
#30931=CARTESIAN_POINT('Ctrl Pts',(1.5143365021986,-1.84878472647799,2.77555756156289E-16));
#30932=CARTESIAN_POINT('Ctrl Pts',(1.46963595841736,-1.87778722506477,2.90023153883192E-16));
#30933=CARTESIAN_POINT('Ctrl Pts',(1.42385657678108,-1.90524929950103,3.23574125955808E-17));
#30934=CARTESIAN_POINT('Ctrl Pts',(1.37702479013104,-1.93106208855763,5.55111512312578E-17));
#30935=CARTESIAN_POINT('Ctrl Pts',(0.261124777554701,2.92529416030267,11.058));
#30936=CARTESIAN_POINT('Ctrl Pts',(0.712806568001128,2.88599464153458,11.0335796606559));
#30937=CARTESIAN_POINT('Ctrl Pts',(1.15551467718148,2.74786827548953,11.0091593213117));
#30938=CARTESIAN_POINT('Ctrl Pts',(1.53904161881194,2.51335023952951,10.9847389819676));
#30939=CARTESIAN_POINT('Ctrl Pts',(2.36167356031087,2.01032944412425,10.9323594774631));
#30940=CARTESIAN_POINT('Ctrl Pts',(2.91203354584656,1.06384412118684,10.8799799729586));
#30941=CARTESIAN_POINT('Ctrl Pts',(2.94465829055491,0.100220893818898,10.8276004684541));
#30942=CARTESIAN_POINT('Ctrl Pts',(2.97728303526326,-0.863402333549067,
10.7752209639496));
#30943=CARTESIAN_POINT('Ctrl Pts',(2.49217253914424,-1.84416346534755,10.7228414594451));
#30944=CARTESIAN_POINT('Ctrl Pts',(1.70632723287924,-2.40227529678238,10.6704619549406));
#30945=CARTESIAN_POINT('Ctrl Pts',(0.92048192661426,-2.96038712821718,10.6180824504361));
#30946=CARTESIAN_POINT('Ctrl Pts',(-0.166098189796688,-3.09584965928835,
10.5657029459315));
#30947=CARTESIAN_POINT('Ctrl Pts',(-1.0650088521454,-2.74748941090806,10.513323441427));
#30948=CARTESIAN_POINT('Ctrl Pts',(-1.96391951449414,-2.39912916252775,
10.4609439369225));
#30949=CARTESIAN_POINT('Ctrl Pts',(-2.67516072278063,-1.56694613469595,
10.408564432418));
#30950=CARTESIAN_POINT('Ctrl Pts',(-2.87955920487239,-0.624834891848815,
10.3561849279135));
#30951=CARTESIAN_POINT('Ctrl Pts',(-2.92379628688831,-0.420937818389941,
10.3448486576389));
#30952=CARTESIAN_POINT('Ctrl Pts',(-2.94429281596354,-0.211891698741057,
10.3335123873642));
#30953=CARTESIAN_POINT('Ctrl Pts',(-2.94242444587263,-0.00248500551853048,
10.3221761170896));
#30954=CARTESIAN_POINT('Origin',(0.,0.,-1.84858989190501));
#30955=CARTESIAN_POINT('',(-1.37702479013099,-1.93106208855767,0.));
#30956=CARTESIAN_POINT('Ctrl Pts',(-1.37989654081094,-1.93326688769301,
3.07371315899641E-16));
#30957=CARTESIAN_POINT('Ctrl Pts',(-0.801986922861967,-2.34019513141193,
0.0475906520026623));
#30958=CARTESIAN_POINT('Ctrl Pts',(0.824868299691477,-2.62988338064349,
0.147626409229032));
#30959=CARTESIAN_POINT('Ctrl Pts',(2.66596861578497,-0.838738147770652,
0.30010727167911));
#30960=CARTESIAN_POINT('Ctrl Pts',(2.16631806184957,1.76615982799916,0.457442587350233));
#30961=CARTESIAN_POINT('Ctrl Pts',(-0.283824062622952,2.78024166545816,
0.614777903021357));
#30962=CARTESIAN_POINT('Ctrl Pts',(-2.10236314538525,1.54689613835291,0.745160337872953));
#30963=CARTESIAN_POINT('Ctrl Pts',(-2.3682722008076,0.381486792202907,0.823097667500842));
#30964=CARTESIAN_POINT('Ctrl Pts',(-2.36802324146013,0.000186122305323062,
0.848589891905023));
#30965=CARTESIAN_POINT('Origin',(0.,0.,0.));
#30966=CARTESIAN_POINT('Ctrl Pts',(-1.03908919352509,2.13201587949044,-0.329233991005384));
#30967=CARTESIAN_POINT('Ctrl Pts',(-1.74163600084562,1.78961280339009,-0.276788885781676));
#30968=CARTESIAN_POINT('Ctrl Pts',(-2.77044124913769,0.362429281341372,
-0.171898675334261));
#30969=CARTESIAN_POINT('Ctrl Pts',(-1.82442757362648,-2.1194917921021,-0.0145633596631371));
#30970=CARTESIAN_POINT('Ctrl Pts',(0.766254154833431,-2.68690713172521,
0.142771956007986));
#30971=CARTESIAN_POINT('Ctrl Pts',(2.66596861578497,-0.838738147770652,
0.30010727167911));
#30972=CARTESIAN_POINT('Ctrl Pts',(2.16631806184957,1.76615982799916,0.457442587350233));
#30973=CARTESIAN_POINT('Ctrl Pts',(-0.283824062622952,2.78024166545816,
0.614777903021357));
#30974=CARTESIAN_POINT('Ctrl Pts',(-2.47829466728951,1.29193683314281,0.772113218692479));
#30975=CARTESIAN_POINT('Ctrl Pts',(-2.44182858239548,-1.35964121596809,
0.929448534363604));
#30976=CARTESIAN_POINT('Ctrl Pts',(-0.207121339063888,-2.78711087979173,
1.08678385003473));
#30977=CARTESIAN_POINT('Ctrl Pts',(2.21401803077907,-1.70561830406782,1.24411916570585));
#30978=CARTESIAN_POINT('Ctrl Pts',(2.64205485235054,0.911349150745493,1.40145448137697));
#30979=CARTESIAN_POINT('Ctrl Pts',(0.691640660298454,2.70787919402874,1.5587897970481));
#30980=CARTESIAN_POINT('Ctrl Pts',(-1.88140253096646,2.06671733364312,1.71612511271922));
#30981=CARTESIAN_POINT('Ctrl Pts',(-2.76076141176456,-0.43496057134077,
1.87346042839035));
#30982=CARTESIAN_POINT('Ctrl Pts',(-1.15481219883121,-2.54507342378116,
2.03079574406147));
#30983=CARTESIAN_POINT('Ctrl Pts',(1.49072764255621,-2.36404822464922,2.18813105973259));
#30984=CARTESIAN_POINT('Ctrl Pts',(2.79427705549031,-0.0548463935276453,
2.34546637540372));
#30985=CARTESIAN_POINT('Ctrl Pts',(1.5823475414007,2.30372918060613,2.50280169107483));
#30986=CARTESIAN_POINT('Ctrl Pts',(-1.05405113312049,2.58842974112365,2.66013700674597));
#30987=CARTESIAN_POINT('Ctrl Pts',(-2.74156638658485,0.542960359863138,
2.81747232241708));
#30988=CARTESIAN_POINT('Ctrl Pts',(-1.9610543025963,-1.99129560121778,2.97480763808821));
#30989=CARTESIAN_POINT('Ctrl Pts',(0.584848394656438,-2.73293698550247,
3.13214295375933));
#30990=CARTESIAN_POINT('Ctrl Pts',(2.60425579784155,-1.01431944186932,3.28947826943046));
#30991=CARTESIAN_POINT('Ctrl Pts',(2.27924634057658,1.61741407950708,3.44681358510158));
#30992=CARTESIAN_POINT('Ctrl Pts',(-0.0975982492034651,2.79311059143494,
3.6041489007727));
#30993=CARTESIAN_POINT('Ctrl Pts',(-2.38658243027454,1.45437838755459,3.76148421644382));
#30994=CARTESIAN_POINT('Ctrl Pts',(-2.52710481755741,-1.19362198012869,
3.91881953211495));
#30995=CARTESIAN_POINT('Ctrl Pts',(-0.392663608746353,-2.76709368867159,
4.07615484778607));
#30996=CARTESIAN_POINT('Ctrl Pts',(2.09526330020315,-1.8495577562663,4.23349016345719));
#30997=CARTESIAN_POINT('Ctrl Pts',(2.69698125586998,0.732996791565816,4.39082547912832));
#30998=CARTESIAN_POINT('Ctrl Pts',(0.870808554093777,2.65568911080063,4.54816079479944));
#30999=CARTESIAN_POINT('Ctrl Pts',(-1.73928800639316,2.18766300463189,4.70549611047057));
#31000=CARTESIAN_POINT('Ctrl Pts',(-2.78363356575401,-0.249752602863106,
4.86283142614169));
#31001=CARTESIAN_POINT('Ctrl Pts',(-1.32208186928512,-2.46233460804071,
5.02016674181281));
#31002=CARTESIAN_POINT('Ctrl Pts',(1.32964132424929,-2.45826079574207,5.17750205748394));
#31003=CARTESIAN_POINT('Ctrl Pts',(2.78438780839412,-0.241198514719961,
5.33483737315506));
#31004=CARTESIAN_POINT('Ctrl Pts',(1.73255804842731,2.19299676239354,5.49217268882618));
#31005=CARTESIAN_POINT('Ctrl Pts',(-0.878964234485193,2.65300095467984,
5.64950800449731));
#31006=CARTESIAN_POINT('Ctrl Pts',(-2.69922070918587,0.72470666765315,5.80684332016843));
#31007=CARTESIAN_POINT('Ctrl Pts',(-2.08957051396587,-1.85598686908106,
5.96417863583956));
#31008=CARTESIAN_POINT('Ctrl Pts',(0.401163844498212,-2.76587414046649,
6.12151395151068));
#31009=CARTESIAN_POINT('Ctrl Pts',(2.53076037597685,-1.18585163930103,6.2788492671818));
#31010=CARTESIAN_POINT('Ctrl Pts',(2.38210248511723,1.46170446446183,6.43618458285292));
#31011=CARTESIAN_POINT('Ctrl Pts',(0.0890157606711408,2.793397283841,6.59351989852405));
#31012=CARTESIAN_POINT('Ctrl Pts',(-2.28420520026003,1.61040330172691,6.75085521419516));
#31013=CARTESIAN_POINT('Ctrl Pts',(-2.60112693645964,-1.02231641451357,
6.9081905298663));
#31014=CARTESIAN_POINT('Ctrl Pts',(-0.57644849505612,-2.73472106868152,
7.06552584553741));
#31015=CARTESIAN_POINT('Ctrl Pts',(1.96716344393165,-1.98526073259378,7.22286116120855));
#31016=CARTESIAN_POINT('Ctrl Pts',(2.73988515609665,0.551381466653972,7.38019647687966));
#31017=CARTESIAN_POINT('Ctrl Pts',(1.04609303646807,2.5916561403346,7.53753179255079));
#31018=CARTESIAN_POINT('Ctrl Pts',(-1.58941846186445,2.2988564868904,7.69486710822191));
#31019=CARTESIAN_POINT('Ctrl Pts',(-2.79409530723714,-0.0634318507917163,
7.85220242389303));
#31020=CARTESIAN_POINT('Ctrl Pts',(-1.48345697628832,-2.36861723168749,
8.00953773956416));
#31021=CARTESIAN_POINT('Ctrl Pts',(1.16262680634646,-2.54151354917186,8.16687305523529));
#31022=CARTESIAN_POINT('Ctrl Pts',(2.76208455499713,-0.426475157784177,
8.3242083709064));
#31023=CARTESIAN_POINT('Ctrl Pts',(1.8750440359881,2.07248692819523,8.48154368657753));
#31024=CARTESIAN_POINT('Ctrl Pts',(-0.699958537943023,2.7057439570526,8.63887900224866));
#31025=CARTESIAN_POINT('Ctrl Pts',(-2.6448406647993,0.903221864868725,8.79621431791976));
#31026=CARTESIAN_POINT('Ctrl Pts',(-2.20877058145475,-1.7124032551425,8.95354963359091));
#31027=CARTESIAN_POINT('Ctrl Pts',(0.215690902196592,-2.78647992051942,
9.11088494926201));
#31028=CARTESIAN_POINT('Ctrl Pts',(2.4459813653409,-1.35209655994371,9.26822026493315));
#31029=CARTESIAN_POINT('Ctrl Pts',(2.47433880171217,1.29947749716991,9.42555558060427));
#31030=CARTESIAN_POINT('Ctrl Pts',(0.275231669725872,2.78123058171878,9.58289089627539));
#31031=CARTESIAN_POINT('Ctrl Pts',(-2.17164161907558,1.7592467736877,9.74022621194653));
#31032=CARTESIAN_POINT('Ctrl Pts',(-2.66355657074516,-0.846449946443288,
9.89756152761763));
#31033=CARTESIAN_POINT('Ctrl Pts',(-0.757654725048104,-2.69016151139635,
10.0548968432888));
#31034=CARTESIAN_POINT('Ctrl Pts',(1.83027666927001,-2.11210170665972,10.2122321589599));
#31035=CARTESIAN_POINT('Ctrl Pts',(2.77060484795253,0.367287133540841,10.369567474631));
#31036=CARTESIAN_POINT('Ctrl Pts',(1.21665350181368,2.51610800548609,10.5269027903021));
#31037=CARTESIAN_POINT('Ctrl Pts',(-1.43234772356642,2.39972494583597,10.6842381059733));
#31038=CARTESIAN_POINT('Ctrl Pts',(-2.79231938150401,0.123316482315984,
10.8415734216444));
#31039=CARTESIAN_POINT('Ctrl Pts',(-1.63779792657952,-2.26461658842463,
10.9989087373155));
#31040=CARTESIAN_POINT('Ctrl Pts',(0.989622905930635,-2.61290295808564,
11.1562440529866));
#31041=CARTESIAN_POINT('Ctrl Pts',(2.72902843688469,-0.61088887604173,11.3135793686578));
#31042=CARTESIAN_POINT('Ctrl Pts',(2.00599839187704,1.9449087769569,11.4709146843289));
#31043=CARTESIAN_POINT('Ctrl Pts',(0.328567026486064,2.47549058867235,11.5758048947763));
#31044=CARTESIAN_POINT('Ctrl Pts',(-0.439445221994061,2.3306835819919,11.62825));
#31045=CARTESIAN_POINT('Ctrl Pts',(-1.12236674703447,2.30288577939268,-0.219489327336923));
#31046=CARTESIAN_POINT('Ctrl Pts',(-1.881218999262,1.93304089110777,-0.167044222113215));
#31047=CARTESIAN_POINT('Ctrl Pts',(-2.9924775967461,0.391476088928602,-0.0621540116657994));
#31048=CARTESIAN_POINT('Ctrl Pts',(-1.97064588273166,-2.28935795203269,
0.0951813040053245));
#31049=CARTESIAN_POINT('Ctrl Pts',(0.82766540978493,-2.90224865758394,0.252516619676447));
#31050=CARTESIAN_POINT('Ctrl Pts',(2.87963202931947,-0.905958614903406,
0.409851935347572));
#31051=CARTESIAN_POINT('Ctrl Pts',(2.33993710190716,1.90770828264466,0.567187251018694));
#31052=CARTESIAN_POINT('Ctrl Pts',(-0.306571073860874,3.00306346507554,
0.724522566689817));
#31053=CARTESIAN_POINT('Ctrl Pts',(-2.67691699735827,1.39547879991837,0.881857882360941));
#31054=CARTESIAN_POINT('Ctrl Pts',(-2.63752834686069,-1.46860933422193,
1.03919319803207));
#31055=CARTESIAN_POINT('Ctrl Pts',(-0.223721028969555,-3.01048321093979,
1.19652851370319));
#31056=CARTESIAN_POINT('Ctrl Pts',(2.39145997337443,-1.84231467283839,1.35386382937431));
#31057=CARTESIAN_POINT('Ctrl Pts',(2.85380170306596,0.984389009248359,1.51119914504543));
#31058=CARTESIAN_POINT('Ctrl Pts',(0.747072034675363,2.92490152077689,1.66853446071656));
#31059=CARTESIAN_POINT('Ctrl Pts',(-2.03218708432488,2.23235389729304,1.82586977638768));
#31060=CARTESIAN_POINT('Ctrl Pts',(-2.98202197113476,-0.469820381720866,
1.98320509205881));
#31061=CARTESIAN_POINT('Ctrl Pts',(-1.24736434476896,-2.74904772122835,
2.14054040772993));
#31062=CARTESIAN_POINT('Ctrl Pts',(1.61020165094208,-2.55351430104939,2.29787572340105));
#31063=CARTESIAN_POINT('Ctrl Pts',(3.01822371806624,-0.0592420445461263,
2.45521103907218));
#31064=CARTESIAN_POINT('Ctrl Pts',(1.70916440454448,2.48836100172844,2.6125463547433));
#31065=CARTESIAN_POINT('Ctrl Pts',(-1.13852780768032,2.79587882019688,2.76988167041443));
#31066=CARTESIAN_POINT('Ctrl Pts',(-2.9612885652785,0.586475787319947,2.92721698608554));
#31067=CARTESIAN_POINT('Ctrl Pts',(-2.11822252803541,-2.15088750826171,
3.08455230175667));
#31068=CARTESIAN_POINT('Ctrl Pts',(0.631720928587459,-2.95196756292179,
3.24188761742779));
#31069=CARTESIAN_POINT('Ctrl Pts',(2.81297325242419,-1.09561182958951,3.39922293309892));
#31070=CARTESIAN_POINT('Ctrl Pts',(2.46191599037299,1.74704134191371,3.55655824877004));
#31071=CARTESIAN_POINT('Ctrl Pts',(-0.105420237413036,3.01696376802969,
3.71389356444116));
#31072=CARTESIAN_POINT('Ctrl Pts',(-2.57785450516496,1.57093919364055,3.87122888011228));
#31073=CARTESIAN_POINT('Ctrl Pts',(-2.72963902538035,-1.28928452665457,
4.02856419578341));
#31074=CARTESIAN_POINT('Ctrl Pts',(-0.424133539231963,-2.98886174685155,
4.18589951145453));
#31075=CARTESIAN_POINT('Ctrl Pts',(2.26318767347756,-1.99779011781522,4.34323482712566));
#31076=CARTESIAN_POINT('Ctrl Pts',(2.91313016998542,0.791742643136777,4.50057014279678));
#31077=CARTESIAN_POINT('Ctrl Pts',(0.940599296228219,2.86852867588043,4.6579054584679));
#31078=CARTESIAN_POINT('Ctrl Pts',(-1.87868282535885,2.36299272999521,4.81524077413902));
#31079=CARTESIAN_POINT('Ctrl Pts',(-3.00672720840483,-0.269768965152914,
4.97257608981016));
#31080=CARTESIAN_POINT('Ctrl Pts',(-1.42803980273229,-2.65967782299944,
5.12991140548127));
#31081=CARTESIAN_POINT('Ctrl Pts',(1.43620510839645,-2.65527751599392,5.28724672115241));
#31082=CARTESIAN_POINT('Ctrl Pts',(3.00754189963992,-0.260529311672868,
5.44458203682351));
#31083=CARTESIAN_POINT('Ctrl Pts',(1.87141349653044,2.36875396048986,5.60191735249465));
#31084=CARTESIAN_POINT('Ctrl Pts',(-0.949408611663097,2.86562507813386,
5.75925266816576));
#31085=CARTESIAN_POINT('Ctrl Pts',(-2.9155491037487,0.782788109236974,5.9165879838369));
#31086=CARTESIAN_POINT('Ctrl Pts',(-2.25703864025646,-2.00473449033026,
6.07392329950801));
#31087=CARTESIAN_POINT('Ctrl Pts',(0.433315024333776,-2.98754445824887,
6.23125861517914));
#31088=CARTESIAN_POINT('Ctrl Pts',(2.73358755765012,-1.28089143373012,6.38859393085026));
#31089=CARTESIAN_POINT('Ctrl Pts',(2.57301551588047,1.57885241721953,6.54592924652138));
#31090=CARTESIAN_POINT('Ctrl Pts',(0.0961499074014511,3.01727343732968,
6.70326456219251));
#31091=CARTESIAN_POINT('Ctrl Pts',(-2.46727227667312,1.73946868703451,6.86059987786364));
#31092=CARTESIAN_POINT('Ctrl Pts',(-2.80959362919934,-1.104249717683,7.01793519353475));
#31093=CARTESIAN_POINT('Ctrl Pts',(-0.622647821053927,-2.95389463101813,
7.17527050920589));
#31094=CARTESIAN_POINT('Ctrl Pts',(2.12482128503379,-2.14436897654329,7.33260582487699));
#31095=CARTESIAN_POINT('Ctrl Pts',(2.95947259297716,0.59557180168919,7.48994114054813));
#31096=CARTESIAN_POINT('Ctrl Pts',(1.12993191128569,2.79936379839662,7.64727645621924));
#31097=CARTESIAN_POINT('Ctrl Pts',(-1.71680202222819,2.4830977871468,7.80461177189038));
#31098=CARTESIAN_POINT('Ctrl Pts',(-3.01802740364303,-0.0685155812177535,
7.96194708756148));
#31099=CARTESIAN_POINT('Ctrl Pts',(-1.60234827887482,-2.55844949005786,
8.11928240323263));
#31100=CARTESIAN_POINT('Ctrl Pts',(1.25580525212405,-2.74520254132467,8.27661771890373));
#31101=CARTESIAN_POINT('Ctrl Pts',(2.98345115736347,-0.460654906735591,
8.43395303457487));
#31102=CARTESIAN_POINT('Ctrl Pts',(2.02531898929576,2.23858589461288,8.591288350246));
#31103=CARTESIAN_POINT('Ctrl Pts',(-0.756056546623237,2.92259515574686,
8.74862366591711));
#31104=CARTESIAN_POINT('Ctrl Pts',(-2.85681078378342,0.975610363999675,
8.90595898158824));
#31105=CARTESIAN_POINT('Ctrl Pts',(-2.38579196848608,-1.84964340218511,
9.06329429725935));
#31106=CARTESIAN_POINT('Ctrl Pts',(0.232977397678477,-3.00980168358836,
9.2206296129305));
#31107=CARTESIAN_POINT('Ctrl Pts',(2.6420139535965,-1.46046001355504,9.37796492860159));
#31108=CARTESIAN_POINT('Ctrl Pts',(2.67264408988566,1.40362380865033,9.53530024427275));
#31109=CARTESIAN_POINT('Ctrl Pts',(0.297290045701602,3.00413163779202,9.69263555994384));
#31110=CARTESIAN_POINT('Ctrl Pts',(-2.34568731434669,1.90024118325806,9.84997087561499));
#31111=CARTESIAN_POINT('Ctrl Pts',(-2.87702667151006,-0.914288473825907,
10.0073061912861));
#31112=CARTESIAN_POINT('Ctrl Pts',(-0.818376780767691,-2.90576385873112,
10.1646415069572));
#31113=CARTESIAN_POINT('Ctrl Pts',(1.97696375273877,-2.2813755899699,10.3219768226283));
#31114=CARTESIAN_POINT('Ctrl Pts',(2.99265430714862,0.396723272524227,10.4793121382995));
#31115=CARTESIAN_POINT('Ctrl Pts',(1.31416190410585,2.71776087645035,10.6366474539706));
#31116=CARTESIAN_POINT('Ctrl Pts',(-1.54714288738549,2.59205032447523,10.7939827696417));
#31117=CARTESIAN_POINT('Ctrl Pts',(-3.01610914676913,0.133199652133039,
10.9513180853128));
#31118=CARTESIAN_POINT('Ctrl Pts',(-1.76905884750739,-2.44611374025332,
11.108653400984));
#31119=CARTESIAN_POINT('Ctrl Pts',(1.06893599571762,-2.82231343724637,11.2659887166551));
#31120=CARTESIAN_POINT('Ctrl Pts',(2.94774576461505,-0.659848418090555,
11.4233240323262));
#31121=CARTESIAN_POINT('Ctrl Pts',(2.1667686505423,2.10078302312668,11.5806593479973));
#31122=CARTESIAN_POINT('Ctrl Pts',(0.35489995180194,2.67388818653474,11.6855495584447));
#31123=CARTESIAN_POINT('Ctrl Pts',(-0.474664453622185,2.51747565713064,
11.7379946636685));
#31124=CARTESIAN_POINT('Ctrl Pts',(-1.20564430054384,2.47375567929493,-0.109744663668461));
#31125=CARTESIAN_POINT('Ctrl Pts',(-2.02080199767838,2.07646897882546,-0.0572995584447534));
#31126=CARTESIAN_POINT('Ctrl Pts',(-3.21451394435451,0.420522896515832,
0.0475906520026618));
#31127=CARTESIAN_POINT('Ctrl Pts',(-2.11686419183683,-2.45922411196328,
0.204925967673786));
#31128=CARTESIAN_POINT('Ctrl Pts',(0.88907666473643,-3.11759018344267,0.362261283344908));
#31129=CARTESIAN_POINT('Ctrl Pts',(3.09329544285396,-0.973179082036162,
0.519596599016033));
#31130=CARTESIAN_POINT('Ctrl Pts',(2.51355614196476,2.04925673729017,0.676931914687155));
#31131=CARTESIAN_POINT('Ctrl Pts',(-0.329318085098797,3.22588526469291,
0.83426723035828));
#31132=CARTESIAN_POINT('Ctrl Pts',(-2.87553932742704,1.49902076669393,0.991602546029402));
#31133=CARTESIAN_POINT('Ctrl Pts',(-2.8332281113259,-1.57757745247578,1.14893786170053));
#31134=CARTESIAN_POINT('Ctrl Pts',(-0.240320718875223,-3.23385554208785,
1.30627317737165));
#31135=CARTESIAN_POINT('Ctrl Pts',(2.5689019159698,-1.97901104160895,1.46360849304277));
#31136=CARTESIAN_POINT('Ctrl Pts',(3.06554855378139,1.05742886775122,1.6209438087139));
#31137=CARTESIAN_POINT('Ctrl Pts',(0.802503409052275,3.14192384752506,1.77827912438502));
#31138=CARTESIAN_POINT('Ctrl Pts',(-2.18297163768331,2.39799046094296,1.93561444005614));
#31139=CARTESIAN_POINT('Ctrl Pts',(-3.20328253050495,-0.504680192100957,
2.09294975572727));
#31140=CARTESIAN_POINT('Ctrl Pts',(-1.33991649070671,-2.95302201867555,
2.25028507139839));
#31141=CARTESIAN_POINT('Ctrl Pts',(1.72967565932795,-2.74298037744955,2.40762038706951));
#31142=CARTESIAN_POINT('Ctrl Pts',(3.24217038064216,-0.0636376955646108,
2.56495570274064));
#31143=CARTESIAN_POINT('Ctrl Pts',(1.83598126768827,2.67299282285076,2.72229101841176));
#31144=CARTESIAN_POINT('Ctrl Pts',(-1.22300448224015,3.00332789927011,2.87962633408289));
#31145=CARTESIAN_POINT('Ctrl Pts',(-3.18101074397215,0.629991214776759,
3.036961649754));
#31146=CARTESIAN_POINT('Ctrl Pts',(-2.27539075347452,-2.31047941530565,
3.19429696542514));
#31147=CARTESIAN_POINT('Ctrl Pts',(0.678593462518484,-3.1709981403411,3.35163228109625));
#31148=CARTESIAN_POINT('Ctrl Pts',(3.02169070700682,-1.1769042173097,3.50896759676738));
#31149=CARTESIAN_POINT('Ctrl Pts',(2.64458564016939,1.87666860432035,3.6663029124385));
#31150=CARTESIAN_POINT('Ctrl Pts',(-0.113242225622608,3.24081694462443,
3.82363822810962));
#31151=CARTESIAN_POINT('Ctrl Pts',(-2.76912658005537,1.68749999972651,3.98097354378075));
#31152=CARTESIAN_POINT('Ctrl Pts',(-2.93217323320329,-1.38494707318046,
4.13830885945187));
#31153=CARTESIAN_POINT('Ctrl Pts',(-0.45560346971757,-3.21062980503151,
4.295644175123));
#31154=CARTESIAN_POINT('Ctrl Pts',(2.43111204675198,-2.14602247936414,4.45297949079412));
#31155=CARTESIAN_POINT('Ctrl Pts',(3.12927908410086,0.850488494707743,4.61031480646524));
#31156=CARTESIAN_POINT('Ctrl Pts',(1.01039003836266,3.08136824096022,4.76765012213636));
#31157=CARTESIAN_POINT('Ctrl Pts',(-2.01807764432454,2.53832245535854,4.92498543780749));
#31158=CARTESIAN_POINT('Ctrl Pts',(-3.22982085105565,-0.289785327442726,
5.08232075347861));
#31159=CARTESIAN_POINT('Ctrl Pts',(-1.53399773617946,-2.85702103795818,
5.23965606914974));
#31160=CARTESIAN_POINT('Ctrl Pts',(1.5427688925436,-2.85229423624577,5.39699138482085));
#31161=CARTESIAN_POINT('Ctrl Pts',(3.23069599088573,-0.279860108625777,
5.55432670049199));
#31162=CARTESIAN_POINT('Ctrl Pts',(2.01026894463356,2.54451115858618,5.7116620161631));
#31163=CARTESIAN_POINT('Ctrl Pts',(-1.019852988841,3.07824920158788,5.86899733183423));
#31164=CARTESIAN_POINT('Ctrl Pts',(-3.13187749831153,0.840869550820803,
6.02633264750535));
#31165=CARTESIAN_POINT('Ctrl Pts',(-2.42450676654705,-2.15348211157947,
6.18366796317648));
#31166=CARTESIAN_POINT('Ctrl Pts',(0.465466204169338,-3.20921477603124,
6.3410032788476));
#31167=CARTESIAN_POINT('Ctrl Pts',(2.93641473932339,-1.3759312281592,6.49833859451872));
#31168=CARTESIAN_POINT('Ctrl Pts',(2.76392854664371,1.69600036997724,6.65567391018985));
#31169=CARTESIAN_POINT('Ctrl Pts',(0.103284054131762,3.24114959081836,6.81300922586097));
#31170=CARTESIAN_POINT('Ctrl Pts',(-2.65033935308621,1.86853407234211,6.97034454153209));
#31171=CARTESIAN_POINT('Ctrl Pts',(-3.01806032193904,-1.18618302085242,
7.12767985720322));
#31172=CARTESIAN_POINT('Ctrl Pts',(-0.668847147051728,-3.17306819335475,
7.28501517287434));
#31173=CARTESIAN_POINT('Ctrl Pts',(2.28247912613591,-2.30347722049279,7.44235048854546));
#31174=CARTESIAN_POINT('Ctrl Pts',(3.17906002985769,0.639762136724403,7.59968580421659));
#31175=CARTESIAN_POINT('Ctrl Pts',(1.2137707861033,3.00707145645863,7.75702111988771));
#31176=CARTESIAN_POINT('Ctrl Pts',(-1.84418558259193,2.66733908740319,7.91435643555884));
#31177=CARTESIAN_POINT('Ctrl Pts',(-3.24195950004891,-0.0735993116437874,
8.07169175122995));
#31178=CARTESIAN_POINT('Ctrl Pts',(-1.7212395814613,-2.74828174842822,8.22902706690109));
#31179=CARTESIAN_POINT('Ctrl Pts',(1.34898369790163,-2.94889153347749,8.38636238257219));
#31180=CARTESIAN_POINT('Ctrl Pts',(3.20481775972981,-0.494834655687006,
8.54369769824334));
#31181=CARTESIAN_POINT('Ctrl Pts',(2.17559394260342,2.40468486103055,8.70103301391445));
#31182=CARTESIAN_POINT('Ctrl Pts',(-0.812154555303452,3.13944635444111,
8.85836832958556));
#31183=CARTESIAN_POINT('Ctrl Pts',(-3.06878090276754,1.04799886313063,9.01570364525671));
#31184=CARTESIAN_POINT('Ctrl Pts',(-2.56281335551741,-1.98688354922771,
9.17303896092782));
#31185=CARTESIAN_POINT('Ctrl Pts',(0.250263893160364,-3.23312344665729,
9.33037427659894));
#31186=CARTESIAN_POINT('Ctrl Pts',(2.83804654185209,-1.56882346716636,9.48770959227006));
#31187=CARTESIAN_POINT('Ctrl Pts',(2.87094937805915,1.50777012013074,9.64504490794121));
#31188=CARTESIAN_POINT('Ctrl Pts',(0.31934842167733,3.22703269386527,9.8023802236123));
#31189=CARTESIAN_POINT('Ctrl Pts',(-2.5197330096178,2.04123559282842,9.95971553928346));
#31190=CARTESIAN_POINT('Ctrl Pts',(-3.09049677227496,-0.982127001208522,
10.1170508549545));
#31191=CARTESIAN_POINT('Ctrl Pts',(-0.879098836487281,-3.1213662060659,
10.2743861706257));
#31192=CARTESIAN_POINT('Ctrl Pts',(2.12365083620754,-2.45064947328008,10.4317214862968));
#31193=CARTESIAN_POINT('Ctrl Pts',(3.2147037663447,0.426159411507612,10.5890568019679));
#31194=CARTESIAN_POINT('Ctrl Pts',(1.41167030639802,2.9194137474146,10.7463921176391));
#31195=CARTESIAN_POINT('Ctrl Pts',(-1.66193805120456,2.78437570311449,10.9037274333102));
#31196=CARTESIAN_POINT('Ctrl Pts',(-3.23989891203425,0.143082821950096,
11.0610627489813));
#31197=CARTESIAN_POINT('Ctrl Pts',(-1.90031976843527,-2.627610892082,11.2183980646524));
#31198=CARTESIAN_POINT('Ctrl Pts',(1.1482490855046,-3.0317239164071,11.3757333803236));
#31199=CARTESIAN_POINT('Ctrl Pts',(3.16646309234541,-0.708807960139384,
11.5330686959947));
#31200=CARTESIAN_POINT('Ctrl Pts',(2.32753890920755,2.25665726929647,11.6904040116658));
#31201=CARTESIAN_POINT('Ctrl Pts',(0.381232877117816,2.87228578439713,11.7952942221132));
#31202=CARTESIAN_POINT('Ctrl Pts',(-0.50988368525031,2.70426773226937,11.8477393273369));
#31203=CARTESIAN_POINT('Ctrl Pts',(-1.28892185405322,2.64462557919718,0.));
#31204=CARTESIAN_POINT('Ctrl Pts',(-2.16038499609476,2.21989706654315,0.0524451052237078));
#31205=CARTESIAN_POINT('Ctrl Pts',(-3.43655029196293,0.449569704103062,
0.157335315671123));
#31206=CARTESIAN_POINT('Ctrl Pts',(-2.26308250094201,-2.62909027189387,
0.314670631342247));
#31207=CARTESIAN_POINT('Ctrl Pts',(0.950487919687924,-3.33293170930141,
0.47200594701337));
#31208=CARTESIAN_POINT('Ctrl Pts',(3.30695885638846,-1.04039954916892,0.629341262684495));
#31209=CARTESIAN_POINT('Ctrl Pts',(2.68717518202235,2.19080519193567,0.786676578355616));
#31210=CARTESIAN_POINT('Ctrl Pts',(-0.352065096336719,3.44870706431028,
0.944011894026741));
#31211=CARTESIAN_POINT('Ctrl Pts',(-3.0741616574958,1.60256273346949,1.10134720969786));
#31212=CARTESIAN_POINT('Ctrl Pts',(-3.02892787579111,-1.68654557072963,
1.25868252536899));
#31213=CARTESIAN_POINT('Ctrl Pts',(-0.256920408780888,-3.45722787323591,
1.41601784104011));
#31214=CARTESIAN_POINT('Ctrl Pts',(2.74634385856517,-2.11570741037952,1.57335315671124));
#31215=CARTESIAN_POINT('Ctrl Pts',(3.27729540449682,1.13046872625408,1.73068847238236));
#31216=CARTESIAN_POINT('Ctrl Pts',(0.857934783429182,3.35894617427322,1.88802378805348));
#31217=CARTESIAN_POINT('Ctrl Pts',(-2.33375619104173,2.56362702459287,2.0453591037246));
#31218=CARTESIAN_POINT('Ctrl Pts',(-3.42454308987515,-0.539540002481048,
2.20269441939573));
#31219=CARTESIAN_POINT('Ctrl Pts',(-1.43246863664446,-3.15699631612275,
2.36002973506685));
#31220=CARTESIAN_POINT('Ctrl Pts',(1.84914966771382,-2.93244645384971,2.51736505073797));
#31221=CARTESIAN_POINT('Ctrl Pts',(3.46611704321809,-0.0680333465830936,
2.6747003664091));
#31222=CARTESIAN_POINT('Ctrl Pts',(1.96279813083206,2.85762464397308,2.83203568208022));
#31223=CARTESIAN_POINT('Ctrl Pts',(-1.30748115679998,3.21077697834334,2.98937099775135));
#31224=CARTESIAN_POINT('Ctrl Pts',(-3.40073292266579,0.673506642233569,
3.14670631342246));
#31225=CARTESIAN_POINT('Ctrl Pts',(-2.43255897891363,-2.47007132234958,
3.3040416290936));
#31226=CARTESIAN_POINT('Ctrl Pts',(0.725465996449509,-3.39002871776042,
3.46137694476471));
#31227=CARTESIAN_POINT('Ctrl Pts',(3.23040816158946,-1.2581966050299,3.61871226043584));
#31228=CARTESIAN_POINT('Ctrl Pts',(2.8272552899658,2.00629586672699,3.77604757610696));
#31229=CARTESIAN_POINT('Ctrl Pts',(-0.12106421383218,3.46467012121918,3.93338289177809));
#31230=CARTESIAN_POINT('Ctrl Pts',(-2.96039865494578,1.80406080581246,4.09071820744921));
#31231=CARTESIAN_POINT('Ctrl Pts',(-3.13470744102623,-1.48060961970634,
4.24805352312033));
#31232=CARTESIAN_POINT('Ctrl Pts',(-0.48707340020318,-3.43239786321147,
4.40538883879146));
#31233=CARTESIAN_POINT('Ctrl Pts',(2.59903642002639,-2.29425484091306,4.56272415446258));
#31234=CARTESIAN_POINT('Ctrl Pts',(3.3454279982163,0.909234346278705,4.7200594701337));
#31235=CARTESIAN_POINT('Ctrl Pts',(1.0801807804971,3.29420780604002,4.87739478580482));
#31236=CARTESIAN_POINT('Ctrl Pts',(-2.15747246329023,2.71365218072187,5.03473010147595));
#31237=CARTESIAN_POINT('Ctrl Pts',(-3.45291449370647,-0.309801689732533,
5.19206541714708));
#31238=CARTESIAN_POINT('Ctrl Pts',(-1.63995566962662,-3.05436425291692,
5.34940073281819));
#31239=CARTESIAN_POINT('Ctrl Pts',(1.64933267669075,-3.04931095649762,5.50673604848933));
#31240=CARTESIAN_POINT('Ctrl Pts',(3.45385008213154,-0.299190905578683,
5.66407136416044));
#31241=CARTESIAN_POINT('Ctrl Pts',(2.14912439273668,2.7202683566825,5.82140667983157));
#31242=CARTESIAN_POINT('Ctrl Pts',(-1.0902973660189,3.2908733250419,5.97874199550268));
#31243=CARTESIAN_POINT('Ctrl Pts',(-3.34820589287437,0.898950992404627,
6.13607731117382));
#31244=CARTESIAN_POINT('Ctrl Pts',(-2.59197489283764,-2.30222973282867,
6.29341262684493));
#31245=CARTESIAN_POINT('Ctrl Pts',(0.497617384004899,-3.43088509381362,
6.45074794251607));
#31246=CARTESIAN_POINT('Ctrl Pts',(3.13924192099666,-1.47097102258828,6.60808325818718));
#31247=CARTESIAN_POINT('Ctrl Pts',(2.95484157740695,1.81314832273494,6.76541857385831));
#31248=CARTESIAN_POINT('Ctrl Pts',(0.110418200862072,3.46502574430704,6.92275388952943));
#31249=CARTESIAN_POINT('Ctrl Pts',(-2.8334064294993,1.9975994576497,7.08008920520056));
#31250=CARTESIAN_POINT('Ctrl Pts',(-3.22652701467874,-1.26811632402185,
7.23742452087168));
#31251=CARTESIAN_POINT('Ctrl Pts',(-0.715046473049532,-3.39224175569136,
7.3947598365428));
#31252=CARTESIAN_POINT('Ctrl Pts',(2.44013696723805,-2.46258546444229,7.55209515221393));
#31253=CARTESIAN_POINT('Ctrl Pts',(3.39864746673821,0.683952471759619,7.70943046788505));
#31254=CARTESIAN_POINT('Ctrl Pts',(1.29760966092091,3.21477911452065,7.86676578355617));
#31255=CARTESIAN_POINT('Ctrl Pts',(-1.97156914295567,2.85158038765959,8.0241010992273));
#31256=CARTESIAN_POINT('Ctrl Pts',(-3.4658915964548,-0.0786830420698247,
8.18143641489842));
#31257=CARTESIAN_POINT('Ctrl Pts',(-1.84013088404779,-2.93811400679859,
8.33877173056954));
#31258=CARTESIAN_POINT('Ctrl Pts',(1.44216214367922,-3.1525805256303,8.49610704624066));
#31259=CARTESIAN_POINT('Ctrl Pts',(3.42618436209615,-0.529014404638419,
8.6534423619118));
#31260=CARTESIAN_POINT('Ctrl Pts',(2.32586889591107,2.57078382744821,8.81077767758291));
#31261=CARTESIAN_POINT('Ctrl Pts',(-0.868252563983666,3.35629755313536,
8.96811299325404));
#31262=CARTESIAN_POINT('Ctrl Pts',(-3.28075102175166,1.12038736226158,9.12544830892515));
#31263=CARTESIAN_POINT('Ctrl Pts',(-2.73983474254873,-2.12412369627032,
9.28278362459629));
#31264=CARTESIAN_POINT('Ctrl Pts',(0.267550388642249,-3.45644520972622,
9.44011894026741));
#31265=CARTESIAN_POINT('Ctrl Pts',(3.03407913010768,-1.67718692077769,9.59745425593853));
#31266=CARTESIAN_POINT('Ctrl Pts',(3.06925466623264,1.61191643161116,9.75478957160966));
#31267=CARTESIAN_POINT('Ctrl Pts',(0.341406797653059,3.4499337499385,9.91212488728077));
#31268=CARTESIAN_POINT('Ctrl Pts',(-2.69377870488891,2.18223000239878,10.0694602029519));
#31269=CARTESIAN_POINT('Ctrl Pts',(-3.30396687303986,-1.04996552859114,
10.226795518623));
#31270=CARTESIAN_POINT('Ctrl Pts',(-0.939820892206868,-3.33696855340067,
10.3841308342941));
#31271=CARTESIAN_POINT('Ctrl Pts',(2.2703379196763,-2.61992335659027,10.5414661499653));
#31272=CARTESIAN_POINT('Ctrl Pts',(3.43675322554079,0.455595550491001,10.6988014656364));
#31273=CARTESIAN_POINT('Ctrl Pts',(1.50917870869019,3.12106661837885,10.8561367813075));
#31274=CARTESIAN_POINT('Ctrl Pts',(-1.77673321502363,2.97670108175376,11.0134720969786));
#31275=CARTESIAN_POINT('Ctrl Pts',(-3.46368867729937,0.152965991767152,
11.1708074126498));
#31276=CARTESIAN_POINT('Ctrl Pts',(-2.03158068936315,-2.80910804391069,
11.3281427283209));
#31277=CARTESIAN_POINT('Ctrl Pts',(1.22756217529158,-3.24113439556783,11.485478043992));
#31278=CARTESIAN_POINT('Ctrl Pts',(3.38518042007578,-0.757767502188211,
11.6428133596631));
#31279=CARTESIAN_POINT('Ctrl Pts',(2.48830916787281,2.41253151546626,11.8001486753343));
#31280=CARTESIAN_POINT('Ctrl Pts',(0.407565802433691,3.07068338225952,11.9050388857817));
#31281=CARTESIAN_POINT('Ctrl Pts',(-0.545102916878434,2.89105980740811,
11.9574839910054));
#31282=CARTESIAN_POINT('Ctrl Pts',(-2.93989309841074,-0.00232834448912937,
10.1778238829104));
#31283=CARTESIAN_POINT('Ctrl Pts',(-2.94219554736775,-0.304542880453153,
10.1941477614813));
#31284=CARTESIAN_POINT('Ctrl Pts',(-2.89923296915434,-0.606119063222061,
10.2104716400522));
#31285=CARTESIAN_POINT('Ctrl Pts',(-2.80824451487588,-0.892433444227729,
10.226795518623));
#31286=CARTESIAN_POINT('Ctrl Pts',(-2.5159182127622,-1.81229987019432,10.2792406238467));
#31287=CARTESIAN_POINT('Ctrl Pts',(-1.72786955248453,-2.5746342117975,10.3316857290704));
#31288=CARTESIAN_POINT('Ctrl Pts',(-0.798818753698492,-2.83629384979735,
10.3841308342941));
#31289=CARTESIAN_POINT('Ctrl Pts',(0.130232045087536,-3.0979534877972,10.4365759395179));
#31290=CARTESIAN_POINT('Ctrl Pts',(1.20028498238192,-2.85893842219374,10.4890210447416));
#31291=CARTESIAN_POINT('Ctrl Pts',(1.92971400200653,-2.22684440487846,10.5414661499653));
#31292=CARTESIAN_POINT('Ctrl Pts',(2.65914302163113,-1.59475038756318,10.593911255189));
#31293=CARTESIAN_POINT('Ctrl Pts',(3.04794812358597,-0.569577418536059,
10.6463563604127));
#31294=CARTESIAN_POINT('Ctrl Pts',(2.92108825508827,0.387254243958792,10.6988014656364));
#31295=CARTESIAN_POINT('Ctrl Pts',(2.79422838659058,1.34408590645364,10.7512465708601));
#31296=CARTESIAN_POINT('Ctrl Pts',(2.15170354764038,2.23257626241624,10.8036916760838));
#31297=CARTESIAN_POINT('Ctrl Pts',(1.28278914087964,2.6527605176267,10.8561367813075));
#31298=CARTESIAN_POINT('Ctrl Pts',(0.413874734118906,3.07294477283715,10.9085818865312));
#31299=CARTESIAN_POINT('Ctrl Pts',(-0.681429240452357,3.02482292729546,
10.9610269917549));
#31300=CARTESIAN_POINT('Ctrl Pts',(-1.51024047145062,2.53013948952684,11.0134720969786));
#31301=CARTESIAN_POINT('Ctrl Pts',(-1.74480463118476,2.39013776105746,11.0283147313191));
#31302=CARTESIAN_POINT('Ctrl Pts',(-1.95802372783935,2.21436813426865,11.0431573656595));
#31303=CARTESIAN_POINT('Ctrl Pts',(-2.14415473270596,2.01243073062332,11.058));
#31304=CARTESIAN_POINT('Ctrl Pts',(-1.37989654081095,-1.933266887693,1.56125112837913E-17));
#31305=CARTESIAN_POINT('Ctrl Pts',(-1.44414345926609,-1.89839188587405,
5.80920822621902E-18));
#31306=CARTESIAN_POINT('Ctrl Pts',(-1.5065284577229,-1.86047032724736,-1.41833741640826E-16));
#31307=CARTESIAN_POINT('Ctrl Pts',(-1.56680444439783,-1.81955553349441,
-1.49186218934005E-16));
#31308=CARTESIAN_POINT('Ctrl Pts',(-1.63448180748404,-1.77361675247786,
-1.62745475426733E-16));
#31309=CARTESIAN_POINT('Ctrl Pts',(-1.69950176926845,-1.72390575990714,
4.47554715783556E-16));
#31310=CARTESIAN_POINT('Ctrl Pts',(-1.76178079551988,-1.6707784873017,5.27355936696949E-16));
#31311=CARTESIAN_POINT('Ctrl Pts',(-1.80277525259689,-1.63580806744237,
5.79884178102324E-16));
#31312=CARTESIAN_POINT('Ctrl Pts',(-1.84258178887229,-1.59935636303953,
9.13682232518509E-17));
#31313=CARTESIAN_POINT('Ctrl Pts',(-1.88117141744704,-1.56151405921777,
1.59594559789866E-16));
#31314=CARTESIAN_POINT('Ctrl Pts',(-1.89157558896771,-1.55131137434519,
1.77989100856589E-16));
#31315=CARTESIAN_POINT('Ctrl Pts',(-1.90188938652621,-1.54100934347453,
3.40635361961997E-16));
#31316=CARTESIAN_POINT('Ctrl Pts',(-1.91210630257196,-1.53061605927472,
3.05311331771918E-16));
#31317=CARTESIAN_POINT('Ctrl Pts',(-1.9724409846318,-1.46923985779222,9.67098202152561E-17));
#31318=CARTESIAN_POINT('Ctrl Pts',(-2.02946085491381,-1.40462521591101,
1.4935214824922E-16));
#31319=CARTESIAN_POINT('Ctrl Pts',(-2.08307562783518,-1.33717477526203,
1.38777878078145E-16));
#31320=CARTESIAN_POINT('Ctrl Pts',(-2.12998855414138,-1.27815563969417,
1.29525391678454E-16));
#31321=CARTESIAN_POINT('Ctrl Pts',(-2.17429437900105,-1.21696417926775,
2.01441503266146E-16));
#31322=CARTESIAN_POINT('Ctrl Pts',(-2.21591583956505,-1.15384057343859,
1.52655665885959E-16));
#31323=CARTESIAN_POINT('Ctrl Pts',(-2.23664963326987,-1.12239545345888,
1.28352927004359E-16));
#31324=CARTESIAN_POINT('Ctrl Pts',(-2.25671701785544,-1.09047047206691,
-2.37280165770185E-16));
#31325=CARTESIAN_POINT('Ctrl Pts',(-2.2761066605572,-1.05809323638609,-2.63677968348475E-16));
#31326=CARTESIAN_POINT('Ctrl Pts',(-2.28578146762193,-1.0419380388242,-2.76849621421526E-16));
#31327=CARTESIAN_POINT('Ctrl Pts',(-2.29528887628369,-1.02566760843717,
-1.10809144900277E-17));
#31328=CARTESIAN_POINT('Ctrl Pts',(-2.30461525834334,-1.0093071858719,0.));
#31329=CARTESIAN_POINT('Ctrl Pts',(-2.34846766322256,-0.932380906234359,
5.21021705459412E-17));
#31330=CARTESIAN_POINT('Ctrl Pts',(-2.38837887518559,-0.853373340579809,
-1.59588577561705E-17));
#31331=CARTESIAN_POINT('Ctrl Pts',(-2.42425706703596,-0.772682188207588,
-2.77555756156289E-17));
#31332=CARTESIAN_POINT('Ctrl Pts',(-2.46075963346513,-0.690586798283878,
-3.97575872863117E-17));
#31333=CARTESIAN_POINT('Ctrl Pts',(-2.49308822244858,-0.606748001409621,
2.24945356107799E-18));
#31334=CARTESIAN_POINT('Ctrl Pts',(-2.52111243497218,-0.521542915861604,
-2.77555756156289E-17));
#31335=CARTESIAN_POINT('Ctrl Pts',(-2.54406484395513,-0.4517581906252,-5.23303143573299E-17));
#31336=CARTESIAN_POINT('Ctrl Pts',(-2.56412941494483,-0.381055975787894,
-5.2234519399031E-17));
#31337=CARTESIAN_POINT('Ctrl Pts',(-2.58121358727312,-0.309628512371508,
-5.55111512312578E-17));
#31338=CARTESIAN_POINT('Ctrl Pts',(-2.59402671651933,-0.256057914809218,
-5.79686251054279E-17));
#31339=CARTESIAN_POINT('Ctrl Pts',(-2.6051630020304,-0.202079063721199,
-1.68485553630616E-16));
#31340=CARTESIAN_POINT('Ctrl Pts',(-2.61457527537642,-0.147769877191515,
-1.94289029309402E-16));
#31341=CARTESIAN_POINT('Ctrl Pts',(-2.617136534184,-0.132991313371873,-2.01310646395843E-16));
#31342=CARTESIAN_POINT('Ctrl Pts',(-2.6195700893165,-0.118188277474481,
-3.31395093795537E-16));
#31343=CARTESIAN_POINT('Ctrl Pts',(-2.6218748923051,-0.103362317982878,
-3.33066907387547E-16));
#31344=CARTESIAN_POINT('Ctrl Pts',(-2.62397146608191,-0.089875821288789,
-3.34587679685255E-16));
#31345=CARTESIAN_POINT('Ctrl Pts',(-2.62596008221826,-0.076379405564125,
-2.78772373994456E-16));
#31346=CARTESIAN_POINT('Ctrl Pts',(-2.62784009463941,-0.0628763941457686,
-2.77555756156289E-16));
#31347=CARTESIAN_POINT('Ctrl Pts',(-2.64060982150785,0.0288409614284714,
-2.69292046128659E-16));
#31348=CARTESIAN_POINT('Ctrl Pts',(-2.64837710873961,0.12089024959815,-1.76997536955934E-16));
#31349=CARTESIAN_POINT('Ctrl Pts',(-2.65101366112809,0.212875307143708,
-1.38777878078145E-16));
#31350=CARTESIAN_POINT('Ctrl Pts',(-2.65226659852151,0.256588270610049,
-1.20615204739669E-16));
#31351=CARTESIAN_POINT('Ctrl Pts',(-2.65236023741492,0.300287183221066,
-4.34987190636111E-16));
#31352=CARTESIAN_POINT('Ctrl Pts',(-2.6512772014093,0.343931535522003,-4.16333634234434E-16));
#31353=CARTESIAN_POINT('Ctrl Pts',(-2.64907421925761,0.432707650667494,
-4.32903459206313E-16));
#31354=CARTESIAN_POINT('Ctrl Pts',(-2.64200629387468,0.521257644934972,
-8.62622134822235E-17));
#31355=CARTESIAN_POINT('Ctrl Pts',(-2.63031624428264,0.609320814221094,
-8.32667268468867E-17));
#31356=CARTESIAN_POINT('Ctrl Pts',(-2.61839797794639,0.699103179787949,
-8.02127613999854E-17));
#31357=CARTESIAN_POINT('Ctrl Pts',(-2.60167524897612,0.788380265268053,
1.49019320792917E-16));
#31358=CARTESIAN_POINT('Ctrl Pts',(-2.58035146554209,0.876878238745711,
2.4980018054066E-16));
#31359=CARTESIAN_POINT('Ctrl Pts',(-2.57698234718955,0.890860754912604,
2.65723370025807E-16));
#31360=CARTESIAN_POINT('Ctrl Pts',(-2.57349826551832,0.904823813068977,
1.71128026421916E-16));
#31361=CARTESIAN_POINT('Ctrl Pts',(-2.56989990586492,0.918766319054272,
1.94289029309402E-16));
#31362=CARTESIAN_POINT('Ctrl Pts',(-2.56629916621592,0.932718046770052,
2.17465351145046E-16));
#31363=CARTESIAN_POINT('Ctrl Pts',(-2.56258611805641,0.946640891227604,
-7.03868084514403E-16));
#31364=CARTESIAN_POINT('Ctrl Pts',(-2.55876298044222,0.960529869852388,
-6.93889390390723E-16));
#31365=CARTESIAN_POINT('Ctrl Pts',(-2.53419843880054,1.04976976342104,-6.29773977327716E-16));
#31366=CARTESIAN_POINT('Ctrl Pts',(-2.50508011125346,1.13766264916498,6.87890529294335E-17));
#31367=CARTESIAN_POINT('Ctrl Pts',(-2.47169823504828,1.22392740477737,8.32667268468867E-17));
#31368=CARTESIAN_POINT('Ctrl Pts',(-2.43767482619284,1.31184999582573,9.80226325947151E-17));
#31369=CARTESIAN_POINT('Ctrl Pts',(-2.39922225163329,1.39808205966622,-2.50151931196036E-16));
#31370=CARTESIAN_POINT('Ctrl Pts',(-2.35659236008881,1.48232869936419,-2.77555756156289E-16));
#31371=CARTESIAN_POINT('Ctrl Pts',(-2.31360056696885,1.56729054124849,-3.05192222745878E-16));
#31372=CARTESIAN_POINT('Ctrl Pts',(-2.26635993703635,1.65023397727082,5.65740922539343E-17));
#31373=CARTESIAN_POINT('Ctrl Pts',(-2.21507658716517,1.73084671943837,5.55111512312578E-17));
#31374=CARTESIAN_POINT('Ctrl Pts',(-2.18435464293681,1.77913880985734,5.48743828668913E-17));
#31375=CARTESIAN_POINT('Ctrl Pts',(-2.15218088295609,1.82659422289983,-3.64380860772878E-16));
#31376=CARTESIAN_POINT('Ctrl Pts',(-2.11859145320912,1.87314213253736,-3.88578058618805E-16));
#31377=CARTESIAN_POINT('Ctrl Pts',(-2.10923966749503,1.88610174750099,-3.95314910385597E-16));
#31378=CARTESIAN_POINT('Ctrl Pts',(-2.09977706809611,1.89899226435558,-9.16981750261902E-17));
#31379=CARTESIAN_POINT('Ctrl Pts',(-2.0902160744712,1.91179680016256,-1.11022302462516E-16));
#31380=CARTESIAN_POINT('Ctrl Pts',(-2.03140899114824,1.99055403331781,-2.29879778669894E-16));
#31381=CARTESIAN_POINT('Ctrl Pts',(-1.96879105165951,2.06618994280669,4.68887291460301E-17));
#31382=CARTESIAN_POINT('Ctrl Pts',(-1.90263522085423,2.13839704217079,0.));
#31383=CARTESIAN_POINT('Ctrl Pts',(-1.83630675569242,2.21079256674222,-4.70110857922477E-17));
#31384=CARTESIAN_POINT('Ctrl Pts',(-1.76642150904269,2.27974226115238,-1.93865480317173E-16));
#31385=CARTESIAN_POINT('Ctrl Pts',(-1.6932045763485,2.34492041918897,-1.66533453693773E-16));
#31386=CARTESIAN_POINT('Ctrl Pts',(-1.62138195170811,2.40885735573024,-1.39721925040515E-16));
#31387=CARTESIAN_POINT('Ctrl Pts',(-1.54635279514513,2.46916580377976,-2.38947154895597E-16));
#31388=CARTESIAN_POINT('Ctrl Pts',(-1.46828869930752,2.52551090354043,-2.77555756156289E-16));
#31389=CARTESIAN_POINT('Ctrl Pts',(-1.41016377964657,2.56746430557163,-3.06302926317174E-16));
#31390=CARTESIAN_POINT('Ctrl Pts',(-1.35035542782446,2.60721994910279,8.78385754915914E-18));
#31391=CARTESIAN_POINT('Ctrl Pts',(-1.28892185405322,2.64462557919718,0.));
#31392=CARTESIAN_POINT('Origin',(0.,0.,0.));
#31393=CARTESIAN_POINT('Origin',(-1.44337567297407,-2.5,-6.));
#31394=CARTESIAN_POINT('',(-1.44337567297407,-2.5,-6.));
#31395=CARTESIAN_POINT('',(1.44337567297406,-2.5,-6.));
#31396=CARTESIAN_POINT('',(-0.721687836487033,-2.5,-6.));
#31397=CARTESIAN_POINT('',(-1.44337567297407,-2.5,-3.));
#31398=CARTESIAN_POINT('',(-1.44337567297407,-2.5,-6.));
#31399=CARTESIAN_POINT('',(1.44337567297406,-2.5,-3.));
#31400=CARTESIAN_POINT('',(-1.44337567297407,-2.5,-3.));
#31401=CARTESIAN_POINT('',(1.44337567297406,-2.5,-6.));
#31402=CARTESIAN_POINT('Origin',(-2.88675134594813,3.53525079574969E-16,
-6.));
#31403=CARTESIAN_POINT('',(-2.88675134594813,3.53525079574969E-16,-6.));
#31404=CARTESIAN_POINT('',(-2.52590742770461,-0.625,-6.));
#31405=CARTESIAN_POINT('',(-2.88675134594813,5.55111512312578E-16,-3.));
#31406=CARTESIAN_POINT('',(-2.88675134594813,3.53525079574969E-16,-6.));
#31407=CARTESIAN_POINT('',(-2.88675134594813,3.53525079574969E-16,-3.));
#31408=CARTESIAN_POINT('Origin',(-1.44337567297406,2.5,-6.));
#31409=CARTESIAN_POINT('',(-1.44337567297406,2.5,-6.));
#31410=CARTESIAN_POINT('',(-1.80421959121758,1.875,-6.));
#31411=CARTESIAN_POINT('',(-1.44337567297406,2.5,-3.));
#31412=CARTESIAN_POINT('',(-1.44337567297406,2.5,-6.));
#31413=CARTESIAN_POINT('',(-1.44337567297406,2.5,-3.));
#31414=CARTESIAN_POINT('Origin',(1.44337567297406,2.5,-6.));
#31415=CARTESIAN_POINT('',(1.44337567297406,2.5,-6.));
#31416=CARTESIAN_POINT('',(0.721687836487033,2.5,-6.));
#31417=CARTESIAN_POINT('',(1.44337567297406,2.5,-3.));
#31418=CARTESIAN_POINT('',(1.44337567297406,2.5,-6.));
#31419=CARTESIAN_POINT('',(1.44337567297406,2.5,-3.));
#31420=CARTESIAN_POINT('Origin',(2.88675134594813,0.,-6.));
#31421=CARTESIAN_POINT('',(2.88675134594813,0.,-6.));
#31422=CARTESIAN_POINT('',(2.52590742770461,0.625,-6.));
#31423=CARTESIAN_POINT('',(2.88675134594813,0.,-3.));
#31424=CARTESIAN_POINT('',(2.88675134594813,0.,-6.));
#31425=CARTESIAN_POINT('',(2.88675134594813,0.,-3.));
#31426=CARTESIAN_POINT('Origin',(1.44337567297406,-2.5,-6.));
#31427=CARTESIAN_POINT('',(1.80421959121758,-1.875,-6.));
#31428=CARTESIAN_POINT('',(1.44337567297406,-2.5,-3.));
#31429=CARTESIAN_POINT('Origin',(0.,0.,-3.));
#31430=CARTESIAN_POINT('Origin',(0.,0.,0.));
#31431=CARTESIAN_POINT('',(-5.,-6.12323399573677E-16,0.));
#31432=CARTESIAN_POINT('Origin',(0.,0.,0.));
#31433=CARTESIAN_POINT('Origin',(0.,0.,-6.));
#31434=CARTESIAN_POINT('',(-5.,-6.12323399573677E-16,-6.));
#31435=CARTESIAN_POINT('',(-5.,-6.12323399573677E-16,-6.));
#31436=CARTESIAN_POINT('Origin',(0.,0.,-6.));
#31437=CARTESIAN_POINT('Origin',(0.,0.,-6.));
#31438=CARTESIAN_POINT('Origin',(0.,0.,12.));
#31439=CARTESIAN_POINT('',(0.,0.,0.));
#31440=CARTESIAN_POINT('Origin',(0.,0.,0.));
#31441=CARTESIAN_POINT('',(-3.5,-4.28626379701574E-16,1.));
#31442=CARTESIAN_POINT('Origin',(0.,0.,1.));
#31443=CARTESIAN_POINT('',(-3.5,-4.28626379701574E-16,0.));
#31444=CARTESIAN_POINT('',(-3.5,-4.28626379701574E-16,0.));
#31445=CARTESIAN_POINT('Origin',(0.,0.,0.));
#31446=CARTESIAN_POINT('Origin',(0.,0.,0.));
#31447=CARTESIAN_POINT('',(-7.,-8.57252759403147E-16,1.));
#31448=CARTESIAN_POINT('Origin',(0.,0.,1.));
#31449=CARTESIAN_POINT('',(-7.,-8.57252759403147E-16,0.));
#31450=CARTESIAN_POINT('',(-7.,-8.57252759403147E-16,0.));
#31451=CARTESIAN_POINT('Origin',(0.,0.,0.));
#31452=CARTESIAN_POINT('Origin',(0.,0.,1.));
#31453=CARTESIAN_POINT('Origin',(0.,0.,0.));
#31454=CARTESIAN_POINT('',(0.,0.,0.));
#31455=CARTESIAN_POINT('Origin',(0.,0.,2.5));
#31456=CARTESIAN_POINT('',(-2.513631052301,-0.000262637959241863,0.387416697508025));
#31457=CARTESIAN_POINT('',(-2.5161395146468,-0.00304292125110089,0.112583302491978));
#31458=CARTESIAN_POINT('',(-2.5175,3.08304831685346E-16,2.5));
#31459=CARTESIAN_POINT('',(-1.91346599666505,1.63598720337496,0.));
#31460=CARTESIAN_POINT('Ctrl Pts',(-2.5161395146468,-0.00304292125110089,
0.112583302491978));
#31461=CARTESIAN_POINT('Ctrl Pts',(-2.51095752260429,0.58940711336228,0.0750555349946524));
#31462=CARTESIAN_POINT('Ctrl Pts',(-2.29922182808405,1.18480356030441,0.0375277674973267));
#31463=CARTESIAN_POINT('Ctrl Pts',(-1.91346599666507,1.63598720337494,7.63278329429795E-16));
#31464=CARTESIAN_POINT('',(1.9169334902101,1.63821054532066,9.12403139361656E-16));
#31465=CARTESIAN_POINT('Origin',(0.,0.,0.));
#31466=CARTESIAN_POINT('Ctrl Pts',(1.91694983752521,1.63822102714878,3.46944695195361E-16));
#31467=CARTESIAN_POINT('Ctrl Pts',(1.40805405000164,2.22926133126499,0.0494979486298783));
#31468=CARTESIAN_POINT('Ctrl Pts',(0.602342674674628,2.56946547367296,0.0989958972597568));
#31469=CARTESIAN_POINT('Ctrl Pts',(-0.175477465753492,2.51505986110806,
0.148493845889635));
#31470=CARTESIAN_POINT('Ctrl Pts',(-0.995235386765838,2.4577208574882,0.200660578729532));
#31471=CARTESIAN_POINT('Ctrl Pts',(-1.7840133645033,1.96207254741093,0.252827311569428));
#31472=CARTESIAN_POINT('Ctrl Pts',(-2.1906858971079,1.24828644590423,0.304994044409325));
#31473=CARTESIAN_POINT('Ctrl Pts',(-2.40486472497323,0.872362678473624,
0.332468262108891));
#31474=CARTESIAN_POINT('Ctrl Pts',(-2.51305801188577,0.435933487418771,
0.359942479808458));
#31475=CARTESIAN_POINT('Ctrl Pts',(-2.513631052301,-0.000262637959241863,
0.387416697508025));
#31476=CARTESIAN_POINT('Origin',(0.,0.,2.5));
#31477=CARTESIAN_POINT('',(-2.52068696412108,-0.00113551940461809,1.38741669750803));
#31478=CARTESIAN_POINT('',(-2.52025742113573,0.00144393706437333,1.11258330249198));
#31479=CARTESIAN_POINT('',(-2.5175,3.08304831685346E-16,2.5));
#31480=CARTESIAN_POINT('Ctrl Pts',(-2.52025742113573,0.00144393706437333,
1.11258330249198));
#31481=CARTESIAN_POINT('Ctrl Pts',(-2.52087167159714,0.0912295143008042,
1.10688933154059));
#31482=CARTESIAN_POINT('Ctrl Pts',(-2.51647663371758,0.180953836073687,
1.10119536058921));
#31483=CARTESIAN_POINT('Ctrl Pts',(-2.50686975205229,0.270115985573038,
1.09550138963782));
#31484=CARTESIAN_POINT('Ctrl Pts',(-2.41885391327537,1.08699722224894,1.04333465679793));
#31485=CARTESIAN_POINT('Ctrl Pts',(-1.89336817952545,1.85669104203942,0.991167923958032));
#31486=CARTESIAN_POINT('Ctrl Pts',(-1.16464801024837,2.23624073783096,0.939001191118135));
#31487=CARTESIAN_POINT('Ctrl Pts',(-0.435927840971309,2.6157904336225,0.886834458278239));
#31488=CARTESIAN_POINT('Ctrl Pts',(0.496026763832904,2.60519600541511,0.834667725438342));
#31489=CARTESIAN_POINT('Ctrl Pts',(1.21582156787348,2.20894038730756,0.782500992598446));
#31490=CARTESIAN_POINT('Ctrl Pts',(1.93561637191406,1.81268476920001,0.73033425975855));
#31491=CARTESIAN_POINT('Ctrl Pts',(2.443251375191,1.03076796119231,0.678167526918654));
#31492=CARTESIAN_POINT('Ctrl Pts',(2.51242958730335,0.212179626056957,0.626000794078758));
#31493=CARTESIAN_POINT('Ctrl Pts',(2.58160779941571,-0.606408709078402,
0.573834061238861));
#31494=CARTESIAN_POINT('Ctrl Pts',(2.21232922036347,-1.46166857134141,0.521667328398964));
#31495=CARTESIAN_POINT('Ctrl Pts',(1.56924485086725,-1.97326693907424,0.469500595559067));
#31496=CARTESIAN_POINT('Ctrl Pts',(0.926160481371042,-2.48486530680706,
0.417333862719171));
#31497=CARTESIAN_POINT('Ctrl Pts',(0.00927032143085621,-2.65280218000971,
0.365167129879276));
#31498=CARTESIAN_POINT('Ctrl Pts',(-0.772843960767751,-2.40046341131198,
0.31300039703938));
#31499=CARTESIAN_POINT('Ctrl Pts',(-1.55495824296637,-2.14812464261425,
0.260833664199484));
#31500=CARTESIAN_POINT('Ctrl Pts',(-2.2022966474234,-1.47551023201612,0.208666931359586));
#31501=CARTESIAN_POINT('Ctrl Pts',(-2.42598179621524,-0.686278012308338,
0.15650019851969));
#31502=CARTESIAN_POINT('Ctrl Pts',(-2.48875205155903,-0.464804623376722,
0.141861233177119));
#31503=CARTESIAN_POINT('Ctrl Pts',(-2.51816092457802,-0.234147943006738,
0.127222267834549));
#31504=CARTESIAN_POINT('Ctrl Pts',(-2.5161395146468,-0.00304292125110089,
0.112583302491978));
#31505=CARTESIAN_POINT('Ctrl Pts',(-2.513631052301,-0.000262637959241863,
0.387416697508025));
#31506=CARTESIAN_POINT('Ctrl Pts',(-2.51414607366698,-0.392294889717208,
0.412109212648355));
#31507=CARTESIAN_POINT('Ctrl Pts',(-2.42773023634316,-0.784138881365407,
0.436801727788684));
#31508=CARTESIAN_POINT('Ctrl Pts',(-2.25319678957557,-1.13170015918752,
0.461494242929014));
#31509=CARTESIAN_POINT('Ctrl Pts',(-1.88446806196691,-1.86597676983647,
0.51366097576891));
#31510=CARTESIAN_POINT('Ctrl Pts',(-1.12244351927786,-2.40260609819826,
0.565827708608806));
#31511=CARTESIAN_POINT('Ctrl Pts',(-0.306910970062746,-2.50259594233506,
0.617994441448702));
#31512=CARTESIAN_POINT('Ctrl Pts',(0.508621579152378,-2.60258578647186,
0.670161174288599));
#31513=CARTESIAN_POINT('Ctrl Pts',(1.37766213489358,-2.26593614638367,0.722327907128496));
#31514=CARTESIAN_POINT('Ctrl Pts',(1.91291169988306,-1.64259837236496,0.774494639968393));
#31515=CARTESIAN_POINT('Ctrl Pts',(2.44816126487255,-1.01926059834626,0.826661372808289));
#31516=CARTESIAN_POINT('Ctrl Pts',(2.64961983911033,-0.109234690397042,
0.878828105648185));
#31517=CARTESIAN_POINT('Ctrl Pts',(2.42745590365758,0.681791395088116,0.930994838488081));
#31518=CARTESIAN_POINT('Ctrl Pts',(2.20529196820482,1.47281748057328,0.983161571327977));
#31519=CARTESIAN_POINT('Ctrl Pts',(1.55950552306154,2.14484374359438,1.03532830416787));
#31520=CARTESIAN_POINT('Ctrl Pts',(0.777965481968195,2.39835160459691,1.08749503700777));
#31521=CARTESIAN_POINT('Ctrl Pts',(-0.00357455912515306,2.65185946559944,
1.13966176984767));
#31522=CARTESIAN_POINT('Ctrl Pts',(-0.920868196168557,2.48684892458339,
1.19182850268756));
#31523=CARTESIAN_POINT('Ctrl Pts',(-1.56505239016155,1.97685639415684,1.24399523552746));
#31524=CARTESIAN_POINT('Ctrl Pts',(-2.15540204953033,1.50948398821232,1.29180238952098));
#31525=CARTESIAN_POINT('Ctrl Pts',(-2.51638244467258,0.752380607759215,
1.3396095435145));
#31526=CARTESIAN_POINT('Ctrl Pts',(-2.52068696412108,-0.00113551940461809,
1.38741669750803));
#31527=CARTESIAN_POINT('Origin',(0.,0.,2.5));
#31528=CARTESIAN_POINT('',(-2.51584480336699,0.00196506899055149,2.38741669750802));
#31529=CARTESIAN_POINT('',(-2.51363229639634,1.41266446666228E-5,2.11258330249198));
#31530=CARTESIAN_POINT('',(-2.5175,3.08304831685346E-16,2.5));
#31531=CARTESIAN_POINT('Ctrl Pts',(-2.51363229639634,1.41266446666228E-5,
2.11258330249198));
#31532=CARTESIAN_POINT('Ctrl Pts',(-2.51365314043488,0.413200028375445,
2.08655639524664));
#31533=CARTESIAN_POINT('Ctrl Pts',(-2.41712296010665,0.826376698454607,
2.0605294880013));
#31534=CARTESIAN_POINT('Ctrl Pts',(-2.22398683849327,1.18795070900901,2.03450258075596));
#31535=CARTESIAN_POINT('Ctrl Pts',(-1.83687666966046,1.91266742746658,1.98233584791606));
#31536=CARTESIAN_POINT('Ctrl Pts',(-1.06166440870055,2.43007701911127,1.93016911507617));
#31537=CARTESIAN_POINT('Ctrl Pts',(-0.243891408049745,2.50955308940395,
1.87800238223627));
#31538=CARTESIAN_POINT('Ctrl Pts',(0.573881592601061,2.58902915969663,1.82583564939637));
#31539=CARTESIAN_POINT('Ctrl Pts',(1.43421533294277,2.23057170863728,1.77366891655648));
#31540=CARTESIAN_POINT('Ctrl Pts',(1.95362700805596,1.59395389183621,1.72150218371658));
#31541=CARTESIAN_POINT('Ctrl Pts',(2.47303868316916,0.957336075035145,1.66933545087668));
#31542=CARTESIAN_POINT('Ctrl Pts',(2.65152829305385,0.0425578924923607,
1.61716871803679));
#31543=CARTESIAN_POINT('Ctrl Pts',(2.40953581913432,-0.742620459122797,
1.56500198519689));
#31544=CARTESIAN_POINT('Ctrl Pts',(2.16754334521479,-1.52779881073796,1.51283525235699));
#31545=CARTESIAN_POINT('Ctrl Pts',(1.50506878749103,-2.1833773314255,1.4606685195171));
#31546=CARTESIAN_POINT('Ctrl Pts',(0.717402890595091,-2.41715770945467,
1.4085017866772));
#31547=CARTESIAN_POINT('Ctrl Pts',(-0.0702630063008448,-2.65093808748384,
1.35633505383731));
#31548=CARTESIAN_POINT('Ctrl Pts',(-0.983120242368966,-2.46292032285465,
1.30416832099741));
#31549=CARTESIAN_POINT('Ctrl Pts',(-1.61427588850106,-1.93687711375941,
1.25200158815751));
#31550=CARTESIAN_POINT('Ctrl Pts',(-2.17654123387562,-1.46825123921249,
1.205528826269));
#31551=CARTESIAN_POINT('Ctrl Pts',(-2.51524406302822,-0.731363410840463,
1.15905606438049));
#31552=CARTESIAN_POINT('Ctrl Pts',(-2.52025742113573,0.00144393706437333,
1.11258330249198));
#31553=CARTESIAN_POINT('Ctrl Pts',(-2.52068696412108,-0.00113551940461809,
1.38741669750803));
#31554=CARTESIAN_POINT('Ctrl Pts',(-2.52107949725397,-0.0698493560164091,
1.3917762763544));
#31555=CARTESIAN_POINT('Ctrl Pts',(-2.51850599021738,-0.138533361798365,
1.39613585520078));
#31556=CARTESIAN_POINT('Ctrl Pts',(-2.51286990332195,-0.206965106428379,
1.40049543404715));
#31557=CARTESIAN_POINT('Ctrl Pts',(-2.4454284715468,-1.02581955675002,1.45266216688705));
#31558=CARTESIAN_POINT('Ctrl Pts',(-1.93947085705393,-1.80855393755627,
1.50482889972694));
#31559=CARTESIAN_POINT('Ctrl Pts',(-1.22052386480191,-2.20627819800367,
1.55699563256684));
#31560=CARTESIAN_POINT('Ctrl Pts',(-0.501576872549894,-2.60400245845108,
1.60916236540673));
#31561=CARTESIAN_POINT('Ctrl Pts',(0.430359497461277,-2.61671659853964,
1.66132909824663));
#31562=CARTESIAN_POINT('Ctrl Pts',(1.15988750019281,-2.2387513379105,1.71349583108653));
#31563=CARTESIAN_POINT('Ctrl Pts',(1.88941550292434,-1.86078607728136,1.76566256392642));
#31564=CARTESIAN_POINT('Ctrl Pts',(2.41653513837623,-1.09214141593451,1.81782929676632));
#31565=CARTESIAN_POINT('Ctrl Pts',(2.50628871104416,-0.27543223888268,1.86999602960622));
#31566=CARTESIAN_POINT('Ctrl Pts',(2.59604228371209,0.541276938169144,1.92216276244611));
#31567=CARTESIAN_POINT('Ctrl Pts',(2.24842979359607,1.40605063092595,1.97432949528601));
#31568=CARTESIAN_POINT('Ctrl Pts',(1.61839553463159,1.93342727280644,2.02649622812591));
#31569=CARTESIAN_POINT('Ctrl Pts',(0.9883612756671,2.46080391468694,2.0786629609658));
#31570=CARTESIAN_POINT('Ctrl Pts',(0.0759052478541385,2.6507835056911,2.1308296938057));
#31571=CARTESIAN_POINT('Ctrl Pts',(-0.712256806761665,2.41868475685738,
2.1829964266456));
#31572=CARTESIAN_POINT('Ctrl Pts',(-1.50041886137746,2.18658600802365,2.23516315948549));
#31573=CARTESIAN_POINT('Ctrl Pts',(-2.16428694279611,1.53240891935204,2.28732989232539));
#31574=CARTESIAN_POINT('Ctrl Pts',(-2.40795002197348,0.747744850575128,
2.33949662516528));
#31575=CARTESIAN_POINT('Ctrl Pts',(-2.48255920772454,0.507482158922327,
2.35546998261286));
#31576=CARTESIAN_POINT('Ctrl Pts',(-2.51777110227279,0.254985358855856,
2.37144334006044));
#31577=CARTESIAN_POINT('Ctrl Pts',(-2.51584480336699,0.00196506899055149,
2.38741669750802));
#31578=CARTESIAN_POINT('Origin',(0.,0.,2.5));
#31579=CARTESIAN_POINT('',(-2.51589013302272,-0.00197902614912163,3.38741669750803));
#31580=CARTESIAN_POINT('',(-2.52021651143941,-0.00144364612508765,3.11258330249198));
#31581=CARTESIAN_POINT('',(-2.5175,3.08304831685346E-16,2.5));
#31582=CARTESIAN_POINT('Ctrl Pts',(-2.52021651143941,-0.00144364612508765,
3.11258330249198));
#31583=CARTESIAN_POINT('Ctrl Pts',(-2.51515411267109,0.729619079365268,
3.06622345895268));
#31584=CARTESIAN_POINT('Ctrl Pts',(-2.17829775808437,1.46475479323487,3.01986361541339));
#31585=CARTESIAN_POINT('Ctrl Pts',(-1.61839525002992,1.93342693235859,2.97350377187409));
#31586=CARTESIAN_POINT('Ctrl Pts',(-0.988361101417928,2.4608034807813,2.9213370390342));
#31587=CARTESIAN_POINT('Ctrl Pts',(-0.0759052345218647,2.65078303997177,
2.8691703061943));
#31588=CARTESIAN_POINT('Ctrl Pts',(0.712256681486064,2.41868433245784,2.81700357335441));
#31589=CARTESIAN_POINT('Ctrl Pts',(1.50041859749399,2.18658562494391,2.76483684051451));
#31590=CARTESIAN_POINT('Ctrl Pts',(2.16428656261379,1.53240865072558,2.71267010767461));
#31591=CARTESIAN_POINT('Ctrl Pts',(2.40794959914724,0.747744719274148,2.66050337483472));
#31592=CARTESIAN_POINT('Ctrl Pts',(2.65161263568068,-0.0369192121772903,
2.60833664199482));
#31593=CARTESIAN_POINT('Ctrl Pts',(2.47507074362777,-0.952070100861841,
2.55616990915492));
#31594=CARTESIAN_POINT('Ctrl Pts',(1.95701531533631,-1.58979072079872,2.50400317631503));
#31595=CARTESIAN_POINT('Ctrl Pts',(1.43895988704484,-2.22751134073559,2.45183644347513));
#31596=CARTESIAN_POINT('Ctrl Pts',(0.579390922514817,-2.5878016919248,2.39966971063523));
#31597=CARTESIAN_POINT('Ctrl Pts',(-0.238549412870579,-2.5100671436653,
2.34750297779534));
#31598=CARTESIAN_POINT('Ctrl Pts',(-1.05648974825598,-2.4323325954058,2.29533624495544));
#31599=CARTESIAN_POINT('Ctrl Pts',(-1.83280145449676,-1.91657314769758,
2.24316951211554));
#31600=CARTESIAN_POINT('Ctrl Pts',(-2.22145326926428,-1.19268150120826,
2.19100277927565));
#31601=CARTESIAN_POINT('Ctrl Pts',(-2.41619980794843,-0.829952222250707,
2.16486295368109));
#31602=CARTESIAN_POINT('Ctrl Pts',(-2.51361136192544,-0.414964391838591,
2.13872312808653));
#31603=CARTESIAN_POINT('Ctrl Pts',(-2.51363229639634,1.41266446666228E-5,
2.11258330249198));
#31604=CARTESIAN_POINT('Ctrl Pts',(-2.51584480336699,0.00196506899055149,
2.38741669750802));
#31605=CARTESIAN_POINT('Ctrl Pts',(-2.51148008169565,-0.571343226589796,
2.42361007290034));
#31606=CARTESIAN_POINT('Ctrl Pts',(-2.31644353295754,-1.14733917999922,
2.45980344829266));
#31607=CARTESIAN_POINT('Ctrl Pts',(-1.95701565897371,-1.58979099958587,
2.49599682368498));
#31608=CARTESIAN_POINT('Ctrl Pts',(-1.43896013986049,-2.22751173208773,
2.54816355652487));
#31609=CARTESIAN_POINT('Ctrl Pts',(-0.579391024697962,-2.58780214820923,
2.60033028936477));
#31610=CARTESIAN_POINT('Ctrl Pts',(0.238549454567511,-2.51006758543924,
2.65249702220466));
#31611=CARTESIAN_POINT('Ctrl Pts',(1.05648993383299,-2.43233302266925,2.70466375504456));
#31612=CARTESIAN_POINT('Ctrl Pts',(1.83280177720141,-1.91657348100776,2.75683048788446));
#31613=CARTESIAN_POINT('Ctrl Pts',(2.22145365982248,-1.19268170883292,2.80899722072435));
#31614=CARTESIAN_POINT('Ctrl Pts',(2.61010554244356,-0.468789936658086,
2.86116395356425));
#31615=CARTESIAN_POINT('Ctrl Pts',(2.61109746431729,0.463234066030113,2.91333068640414));
#31616=CARTESIAN_POINT('Ctrl Pts',(2.22398722823793,1.18795091427809,2.96549741924404));
#31617=CARTESIAN_POINT('Ctrl Pts',(1.83687699215856,1.91266776252607,3.01766415208394));
#31618=CARTESIAN_POINT('Ctrl Pts',(1.06166459812611,2.43007745633383,3.06983088492383));
#31619=CARTESIAN_POINT('Ctrl Pts',(0.243891452474371,2.50955353617875,3.12199761776373));
#31620=CARTESIAN_POINT('Ctrl Pts',(-0.573881693177372,2.58902961602367,
3.17416435060363));
#31621=CARTESIAN_POINT('Ctrl Pts',(-1.4342155904484,2.23057208190574,3.22633108344352));
#31622=CARTESIAN_POINT('Ctrl Pts',(-1.95362735417331,1.59395416098643,3.27849781628342));
#31623=CARTESIAN_POINT('Ctrl Pts',(-2.31512049434143,1.1508894724433,3.31480411002495));
#31624=CARTESIAN_POINT('Ctrl Pts',(-2.5114814387863,0.573092447932525,3.35111040376649));
#31625=CARTESIAN_POINT('Ctrl Pts',(-2.51589013302272,-0.00197902614912163,
3.38741669750803));
#31626=CARTESIAN_POINT('Origin',(0.,0.,2.5));
#31627=CARTESIAN_POINT('',(-2.52065797473119,0.00106685237120291,4.38741669750802));
#31628=CARTESIAN_POINT('',(-2.51644348201823,0.00207613456667446,4.11258330249198));
#31629=CARTESIAN_POINT('',(-2.5175,3.08304831685346E-16,2.5));
#31630=CARTESIAN_POINT('',(1.91346599666507,1.63598720337493,5.));
#31631=CARTESIAN_POINT('Ctrl Pts',(-2.52065797473119,0.00106685237120291,
4.38741669750802));
#31632=CARTESIAN_POINT('Ctrl Pts',(-2.51627582008385,-0.750533596725348,
4.43511093315233));
#31633=CARTESIAN_POINT('Ctrl Pts',(-2.1571958584412,-1.50553160271072,4.48280516879663));
#31634=CARTESIAN_POINT('Ctrl Pts',(-1.56924561797524,-1.97326800927033,
4.53049940444093));
#31635=CARTESIAN_POINT('Ctrl Pts',(-0.926160710476491,-2.48486610557827,
4.58266613728083));
#31636=CARTESIAN_POINT('Ctrl Pts',(-0.00926858752154605,-2.65280097461769,
4.63483287012073));
#31637=CARTESIAN_POINT('Ctrl Pts',(0.772845077643461,-2.40046275794039,
4.68699960296062));
#31638=CARTESIAN_POINT('Ctrl Pts',(1.55495874280847,-2.14812454126309,4.73916633580052));
#31639=CARTESIAN_POINT('Ctrl Pts',(2.20229395018354,-1.47551323886906,4.79133306864041));
#31640=CARTESIAN_POINT('Ctrl Pts',(2.42597897401485,-0.686281044499074,
4.84349980148031));
#31641=CARTESIAN_POINT('Ctrl Pts',(2.64966399784617,0.102951149870913,4.89566653432021));
#31642=CARTESIAN_POINT('Ctrl Pts',(2.44969883813372,1.00880423621685,4.9478332671601));
#31643=CARTESIAN_POINT('Ctrl Pts',(1.91346599666506,1.63598720337495,5.));
#31644=CARTESIAN_POINT('',(-1.91693299680257,1.63821185741719,5.));
#31645=CARTESIAN_POINT('Origin',(0.,0.,5.));
#31646=CARTESIAN_POINT('Ctrl Pts',(-1.91694926235926,1.6382222944622,5.));
#31647=CARTESIAN_POINT('Ctrl Pts',(-1.40805335272935,2.22926302987767,4.95050205137012));
#31648=CARTESIAN_POINT('Ctrl Pts',(-0.602342425840394,2.56946465859549,
4.90100410274024));
#31649=CARTESIAN_POINT('Ctrl Pts',(0.175477439781852,2.51505854463557,4.85150615411036));
#31650=CARTESIAN_POINT('Ctrl Pts',(0.995235071171573,2.45771901258696,4.79933942127047));
#31651=CARTESIAN_POINT('Ctrl Pts',(1.78401295214682,1.96207240922004,4.74717268843057));
#31652=CARTESIAN_POINT('Ctrl Pts',(2.19068546260575,1.2482867574395,4.69500595559068));
#31653=CARTESIAN_POINT('Ctrl Pts',(2.59735797306467,0.534501105658956,4.64283922275078));
#31654=CARTESIAN_POINT('Ctrl Pts',(2.62192511300726,-0.397423594535204,
4.59067248991088));
#31655=CARTESIAN_POINT('Ctrl Pts',(2.25319644256834,-1.13170027426973,4.53850575707098));
#31656=CARTESIAN_POINT('Ctrl Pts',(1.88446777212942,-1.86597695400425,4.48633902423109));
#31657=CARTESIAN_POINT('Ctrl Pts',(1.12244329130898,-2.40260561327913,4.43417229139119));
#31658=CARTESIAN_POINT('Ctrl Pts',(0.306910879222839,-2.50259532036743,
4.3820055585513));
#31659=CARTESIAN_POINT('Ctrl Pts',(-0.508621532863308,-2.60258502745572,
4.3298388257114));
#31660=CARTESIAN_POINT('Ctrl Pts',(-1.37766187621516,-2.26593578235743,
4.2776720928715));
#31661=CARTESIAN_POINT('Ctrl Pts',(-1.91291133870635,-1.64259818874412,
4.22550536003161));
#31662=CARTESIAN_POINT('Ctrl Pts',(-2.29911832868587,-1.19283157963813,
4.18786467418506));
#31663=CARTESIAN_POINT('Ctrl Pts',(-2.51154433642508,-0.59380690010991,
4.15022398833852));
#31664=CARTESIAN_POINT('Ctrl Pts',(-2.51644348201823,0.00207613456667446,
4.11258330249198));
#31665=CARTESIAN_POINT('Origin',(0.,0.,7.20842344717746));
#31666=CARTESIAN_POINT('',(-3.07686640868348,0.00176283637231212,0.791576552822548));
#31667=CARTESIAN_POINT('',(-3.06877657964135,-0.000320642608852016,0.708423447177458));
#31668=CARTESIAN_POINT('',(-3.0735,2.32747228194194E-14,7.20842344717746));
#31669=CARTESIAN_POINT('',(0.793799282532827,-2.96922295374571,0.));
#31670=CARTESIAN_POINT('Ctrl Pts',(-3.06877657964135,-0.000320642608851972,
0.708423447177458));
#31671=CARTESIAN_POINT('Ctrl Pts',(-3.06807698094575,0.532211151373012,
0.680949229477891));
#31672=CARTESIAN_POINT('Ctrl Pts',(-2.68518598576605,2.07671369914706,0.601308278938428));
#31673=CARTESIAN_POINT('Ctrl Pts',(-0.25205435815242,3.60563262622145,0.469500595559067));
#31674=CARTESIAN_POINT('Ctrl Pts',(2.8638258713055,2.21030524695087,0.313000397039378));
#31675=CARTESIAN_POINT('Ctrl Pts',(3.4222759216869,-1.16283315864926,0.15650019851969));
#31676=CARTESIAN_POINT('Ctrl Pts',(1.76703113798771,-2.70903678361537,0.0521667328398966));
#31677=CARTESIAN_POINT('Ctrl Pts',(0.793799282532827,-2.96922295374571,
0.));
#31678=CARTESIAN_POINT('',(-0.795749017144049,-2.97385877393435,2.61949253457777E-15));
#31679=CARTESIAN_POINT('Origin',(0.,0.,0.));
#31680=CARTESIAN_POINT('Ctrl Pts',(-3.07686640868348,0.00176283637231189,
0.791576552822548));
#31681=CARTESIAN_POINT('Ctrl Pts',(-3.07761631882972,0.111377919445277,
0.785882581871163));
#31682=CARTESIAN_POINT('Ctrl Pts',(-3.02309142539902,1.22449894749353,0.728021878079882));
#31683=CARTESIAN_POINT('Ctrl Pts',(-1.66998478533906,3.20643252148329,0.617994441448703));
#31684=CARTESIAN_POINT('Ctrl Pts',(1.74335679702331,3.1676297706248,0.461494242929015));
#31685=CARTESIAN_POINT('Ctrl Pts',(3.60260150316633,0.3038109312067,0.304994044409326));
#31686=CARTESIAN_POINT('Ctrl Pts',(2.27315994968988,-2.77521413120327,0.151162630099654));
#31687=CARTESIAN_POINT('Ctrl Pts',(0.124975895037349,-3.21660834551288,
0.0494979486298794));
#31688=CARTESIAN_POINT('Ctrl Pts',(-0.795758164394602,-2.97388052305263,
9.44882193321117E-16));
#31689=CARTESIAN_POINT('Origin',(0.,0.,7.20842344717746));
#31690=CARTESIAN_POINT('',(-3.06877809850016,1.72465709349923E-5,1.79157655282255));
#31691=CARTESIAN_POINT('',(-3.0773908179647,-0.00138630343203515,1.70842344717746));
#31692=CARTESIAN_POINT('',(-3.0735,2.32747228194194E-14,7.20842344717746));
#31693=CARTESIAN_POINT('Ctrl Pts',(-3.0773908179647,-0.00138630343203517,
1.70842344717746));
#31694=CARTESIAN_POINT('Ctrl Pts',(-3.07213562808389,0.918546890942566,
1.66061629318394));
#31695=CARTESIAN_POINT('Ctrl Pts',(-2.15053865242723,2.85146124051564,1.56064240635052));
#31696=CARTESIAN_POINT('Ctrl Pts',(1.11551761111489,3.4389870765969,1.4085017866772));
#31697=CARTESIAN_POINT('Ctrl Pts',(3.48075054753741,0.977649178608381,1.25200158815752));
#31698=CARTESIAN_POINT('Ctrl Pts',(2.74289601575609,-2.35537719050612,1.09550138963782));
#31699=CARTESIAN_POINT('Ctrl Pts',(-0.440018957118456,-3.58837739167123,
0.939001191118136));
#31700=CARTESIAN_POINT('Ctrl Pts',(-2.74101688880118,-1.96797948390379,
0.809975210298013));
#31701=CARTESIAN_POINT('Ctrl Pts',(-3.06940534554735,-0.47893479386132,
0.733115962317788));
#31702=CARTESIAN_POINT('Ctrl Pts',(-3.06877657964135,-0.000320642608851972,
0.708423447177458));
#31703=CARTESIAN_POINT('Ctrl Pts',(-3.06877809850016,1.72465709353392E-5,
1.79157655282255));
#31704=CARTESIAN_POINT('Ctrl Pts',(-3.06880354602845,0.504456916469473,
1.76554964557721));
#31705=CARTESIAN_POINT('Ctrl Pts',(-2.71474447759704,2.01993058914264,1.68735600549197));
#31706=CARTESIAN_POINT('Ctrl Pts',(-0.349716256635896,3.59845088308181,
1.55699563256684));
#31707=CARTESIAN_POINT('Ctrl Pts',(2.8013094644448,2.28557822072128,1.40049543404715));
#31708=CARTESIAN_POINT('Ctrl Pts',(3.45503873870173,-1.0648536490447,1.24399523552746));
#31709=CARTESIAN_POINT('Ctrl Pts',(1.02868455419652,-3.46595066989846,1.08749503700777));
#31710=CARTESIAN_POINT('Ctrl Pts',(-2.1930684252685,-2.80237835053392,0.936688809439468));
#31711=CARTESIAN_POINT('Ctrl Pts',(-3.07074583027496,-0.892887961556386,
0.83804931471106));
#31712=CARTESIAN_POINT('Ctrl Pts',(-3.07686640868348,0.00176283637231189,
0.791576552822548));
#31713=CARTESIAN_POINT('Origin',(0.,0.,7.20842344717746));
#31714=CARTESIAN_POINT('',(-3.0768164639162,-0.00176248117795978,2.79157655282255));
#31715=CARTESIAN_POINT('',(-3.07147924653364,0.00239906238030041,2.70842344717746));
#31716=CARTESIAN_POINT('',(-3.0735,2.32747228194194E-14,7.20842344717746));
#31717=CARTESIAN_POINT('Ctrl Pts',(-3.07147924653364,0.00239906238030076,
2.70842344717746));
#31718=CARTESIAN_POINT('Ctrl Pts',(-3.07383097630006,0.311299900871277,
2.69245008972988));
#31719=CARTESIAN_POINT('Ctrl Pts',(-2.89044774320411,1.62630098606235,2.6243099994424));
#31720=CARTESIAN_POINT('Ctrl Pts',(-1.02130638419203,3.46815705171515,2.50400317631503));
#31721=CARTESIAN_POINT('Ctrl Pts',(2.32062044975012,2.77234500847627,2.34750297779534));
#31722=CARTESIAN_POINT('Ctrl Pts',(3.59377276955738,-0.394942313892847,
2.19100277927565));
#31723=CARTESIAN_POINT('Ctrl Pts',(1.66316438874938,-3.21015109242256,2.03450258075596));
#31724=CARTESIAN_POINT('Ctrl Pts',(-1.7501104075517,-3.16358476523821,1.87800238223627));
#31725=CARTESIAN_POINT('Ctrl Pts',(-3.03713246509983,-1.17251597915295,
1.7693093377101));
#31726=CARTESIAN_POINT('Ctrl Pts',(-3.0778700436187,-0.0852758672160755,
1.71278302602383));
#31727=CARTESIAN_POINT('Ctrl Pts',(-3.0773908179647,-0.00138630343203517,
1.70842344717746));
#31728=CARTESIAN_POINT('Ctrl Pts',(-3.0768164639162,-0.00176248117795985,
2.79157655282255));
#31729=CARTESIAN_POINT('Ctrl Pts',(-3.0706360140197,0.890758387459429,2.74521670928325));
#31730=CARTESIAN_POINT('Ctrl Pts',(-2.19661894703825,2.79816239430364,2.64669013290406));
#31731=CARTESIAN_POINT('Ctrl Pts',(1.02130620401276,3.46815644429995,2.49599682368497));
#31732=CARTESIAN_POINT('Ctrl Pts',(3.45276382958855,1.07219267437738,2.33949662516528));
#31733=CARTESIAN_POINT('Ctrl Pts',(2.8061681927767,-2.27960425476498,2.18299642664559));
#31734=CARTESIAN_POINT('Ctrl Pts',(-0.34205648942751,-3.59919002761108,
2.02649622812591));
#31735=CARTESIAN_POINT('Ctrl Pts',(-2.71249040954675,-2.02434105954679,
1.89602293685156));
#31736=CARTESIAN_POINT('Ctrl Pts',(-3.06875254056717,-0.506610946699481,
1.8177163784171));
#31737=CARTESIAN_POINT('Ctrl Pts',(-3.06877809850016,1.72465709353392E-5,
1.79157655282255));
#31738=CARTESIAN_POINT('Origin',(0.,0.,7.20842344717746));
#31739=CARTESIAN_POINT('',(-3.0722101457728,0.00253465723558749,3.79157655282255));
#31740=CARTESIAN_POINT('',(-3.07153458742615,-0.00241610203352894,3.70842344717746));
#31741=CARTESIAN_POINT('',(-3.0735,2.32747228194194E-14,7.20842344717746));
#31742=CARTESIAN_POINT('Ctrl Pts',(-3.07153458742615,-0.00241610203352869,
3.70842344717746));
#31743=CARTESIAN_POINT('Ctrl Pts',(-3.06615221533653,0.699662219948585,
3.67211715343592));
#31744=CARTESIAN_POINT('Ctrl Pts',(-2.48197069074528,2.41863106906089,3.58364412685449));
#31745=CARTESIAN_POINT('Ctrl Pts',(0.349716325434694,3.59845154159293,3.44300436743317));
#31746=CARTESIAN_POINT('Ctrl Pts',(3.18897983255535,1.70340642470933,3.28650416891347));
#31747=CARTESIAN_POINT('Ctrl Pts',(3.18534685712864,-1.71018933171035,3.13000397039378));
#31748=CARTESIAN_POINT('Ctrl Pts',(0.342056548577105,-3.59919066394061,
2.9735037718741));
#31749=CARTESIAN_POINT('Ctrl Pts',(-2.48484176394183,-2.41428958805909,
2.83297693080198));
#31750=CARTESIAN_POINT('Ctrl Pts',(-3.06615055852694,-0.697526676037249,
2.74461682256977));
#31751=CARTESIAN_POINT('Ctrl Pts',(-3.07147924653364,0.00239906238030076,
2.70842344717746));
#31752=CARTESIAN_POINT('Ctrl Pts',(-3.0722101457728,0.00253465723558725,
3.79157655282255));
#31753=CARTESIAN_POINT('Ctrl Pts',(-3.0745183487722,0.283281367407046,3.77705050582919));
#31754=CARTESIAN_POINT('Ctrl Pts',(-2.91187546114467,1.56963838731655,3.71035772599594));
#31755=CARTESIAN_POINT('Ctrl Pts',(-1.11551737463701,3.43898632522653,3.5914982133228));
#31756=CARTESIAN_POINT('Ctrl Pts',(2.24412684766706,2.83462531411003,3.43499801480311));
#31757=CARTESIAN_POINT('Ctrl Pts',(3.60321095550619,-0.296771509319279,
3.27849781628342));
#31758=CARTESIAN_POINT('Ctrl Pts',(1.75011009124083,-3.16358418358746,3.12199761776373));
#31759=CARTESIAN_POINT('Ctrl Pts',(-1.66316409145381,-3.2101505430571,2.96549741924404));
#31760=CARTESIAN_POINT('Ctrl Pts',(-3.02187071265548,-1.22888761088956,
2.85535706426364));
#31761=CARTESIAN_POINT('Ctrl Pts',(-3.07759060777944,-0.113556859393683,
2.79738344212315));
#31762=CARTESIAN_POINT('Ctrl Pts',(-3.0768164639162,-0.00176248117795985,
2.79157655282255));
#31763=CARTESIAN_POINT('Origin',(0.,0.,7.20842344717746));
#31764=CARTESIAN_POINT('',(-3.07018609065268,-0.00333738419709156,4.79157655282255));
#31765=CARTESIAN_POINT('',(-3.07735542615147,0.00130247100806778,4.70842344717746));
#31766=CARTESIAN_POINT('',(-3.0735,2.32747228194194E-14,7.20842344717746));
#31767=CARTESIAN_POINT('',(-0.793799282532885,-2.96922295374569,5.));
#31768=CARTESIAN_POINT('Ctrl Pts',(-0.793799282532885,-2.96922295374569,
5.));
#31769=CARTESIAN_POINT('Ctrl Pts',(-1.76703113798775,-2.70903678361534,
4.9478332671601));
#31770=CARTESIAN_POINT('Ctrl Pts',(-2.8692411723445,-1.67944397566504,4.87835878476762));
#31771=CARTESIAN_POINT('Ctrl Pts',(-3.07242022864685,-0.338323361726583,
4.80888430237514));
#31772=CARTESIAN_POINT('Ctrl Pts',(-3.07018609065268,-0.00333738419709143,
4.79157655282255));
#31773=CARTESIAN_POINT('',(0.795750420935782,-2.97385779503552,5.));
#31774=CARTESIAN_POINT('Origin',(0.,0.,5.));
#31775=CARTESIAN_POINT('Ctrl Pts',(0.795759619474687,-2.97387964574988,
5.));
#31776=CARTESIAN_POINT('Ctrl Pts',(-0.124974018843371,-3.21660711871812,
4.95050205137012));
#31777=CARTESIAN_POINT('Ctrl Pts',(-2.17865809628841,-2.79463535584754,
4.85330986709594));
#31778=CARTESIAN_POINT('Ctrl Pts',(-3.0720054550259,-0.916291960093509,
4.75611768282176));
#31779=CARTESIAN_POINT('Ctrl Pts',(-3.07735542615147,0.00130247100806802,
4.70842344717746));
#31780=CARTESIAN_POINT('Origin',(0.,0.,7.20842344717746));
#31781=CARTESIAN_POINT('Ctrl Pts',(-3.07735542615147,0.00130247100806811,
4.70842344717746));
#31782=CARTESIAN_POINT('Ctrl Pts',(-3.07785711635642,0.0873493163837036,
4.70395094998186));
#31783=CARTESIAN_POINT('Ctrl Pts',(-3.03598706278426,1.17657551893794,4.64731171994637));
#31784=CARTESIAN_POINT('Ctrl Pts',(-1.74335774093941,3.16762915537798,4.53850575707099));
#31785=CARTESIAN_POINT('Ctrl Pts',(1.66998541626837,3.20643379740356,4.3820055585513));
#31786=CARTESIAN_POINT('Ctrl Pts',(3.59460935228705,0.387380778120988,4.22550536003161));
#31787=CARTESIAN_POINT('Ctrl Pts',(2.31471223100892,-2.77732417593505,4.06900516151192));
#31788=CARTESIAN_POINT('Ctrl Pts',(-1.02868478492208,-3.46595142305511,
3.91250496299223));
#31789=CARTESIAN_POINT('Ctrl Pts',(-2.89215223470734,-1.62188152779685,
3.79231105821408));
#31790=CARTESIAN_POINT('Ctrl Pts',(-3.07388588181438,-0.309119687570202,
3.72428388627582));
#31791=CARTESIAN_POINT('Ctrl Pts',(-3.07153458742615,-0.00241610203352869,
3.70842344717746));
#31792=CARTESIAN_POINT('Ctrl Pts',(-3.07018609065268,-0.00333738419709143,
4.79157655282255));
#31793=CARTESIAN_POINT('Ctrl Pts',(-3.06568638497092,0.671347129621605,
4.75671756953524));
#31794=CARTESIAN_POINT('Ctrl Pts',(-2.51923155566346,2.36462266851063,4.66969185340803));
#31795=CARTESIAN_POINT('Ctrl Pts',(0.252054090990421,3.60562829022214,4.53049940444094));
#31796=CARTESIAN_POINT('Ctrl Pts',(3.14100203598835,1.79029184281612,4.37399920592124));
#31797=CARTESIAN_POINT('Ctrl Pts',(3.23098071080095,-1.62294021205589,4.21749900740156));
#31798=CARTESIAN_POINT('Ctrl Pts',(0.440018754334274,-3.58837598279832,
4.06099880888186));
#31799=CARTESIAN_POINT('Ctrl Pts',(-2.44746347564723,-2.46982179783519,
3.91902465735553));
#31800=CARTESIAN_POINT('Ctrl Pts',(-3.06622900417178,-0.724951542199748,
3.82921723866909));
#31801=CARTESIAN_POINT('Ctrl Pts',(-3.0722101457728,0.00253465723558725,
3.79157655282255));
#31802=CARTESIAN_POINT('Ctrl Pts',(1.91346599666506,1.63598720337495,5.));
#31803=CARTESIAN_POINT('Ctrl Pts',(2.44969883813372,1.00880423621685,4.9478332671601));
#31804=CARTESIAN_POINT('Ctrl Pts',(2.84962915755861,-0.802901936475035,
4.84349980148031));
#31805=CARTESIAN_POINT('Ctrl Pts',(0.907623535433406,-2.82073584365711,
4.68699960296062));
#31806=CARTESIAN_POINT('Ctrl Pts',(-1.84305283343144,-2.31693123653885,
4.53049940444093));
#31807=CARTESIAN_POINT('Ctrl Pts',(-2.95088590955911,0.248852734190564,
4.37399920592124));
#31808=CARTESIAN_POINT('Ctrl Pts',(-1.42798214179762,2.59460107325983,4.21749900740156));
#31809=CARTESIAN_POINT('Ctrl Pts',(1.36788296256894,2.62638590693459,4.06099880888186));
#31810=CARTESIAN_POINT('Ctrl Pts',(2.94434001769405,0.317303110108862,3.90449861036218));
#31811=CARTESIAN_POINT('Ctrl Pts',(1.89597788891003,-2.27490275351114,3.74799841184249));
#31812=CARTESIAN_POINT('Ctrl Pts',(-0.842594418754297,-2.8389564690227,
3.5914982133228));
#31813=CARTESIAN_POINT('Ctrl Pts',(-2.83001837825583,-0.872220375374214,
3.43499801480311));
#31814=CARTESIAN_POINT('Ctrl Pts',(-2.29454948771943,1.8721145477878,3.27849781628342));
#31815=CARTESIAN_POINT('Ctrl Pts',(0.286452204093653,2.9474871501416,3.12199761776373));
#31816=CARTESIAN_POINT('Ctrl Pts',(2.61208938619102,1.39525806871831,2.96549741924404));
#31817=CARTESIAN_POINT('Ctrl Pts',(2.60911362056983,-1.40081393934628,2.80899722072436));
#31818=CARTESIAN_POINT('Ctrl Pts',(0.280178090464571,-2.94809256433073,
2.65249702220466));
#31819=CARTESIAN_POINT('Ctrl Pts',(-2.29852925502302,-1.86722131596623,
2.49599682368498));
#31820=CARTESIAN_POINT('Ctrl Pts',(-2.82815502421476,0.878231830680435,
2.33949662516528));
#31821=CARTESIAN_POINT('Ctrl Pts',(-0.83655077995882,2.84076309669526,2.1829964266456));
#31822=CARTESIAN_POINT('Ctrl Pts',(1.90081730348005,2.27082432368278,2.02649622812591));
#31823=CARTESIAN_POINT('Ctrl Pts',(2.94365477382811,-0.323496754587683,
1.86999602960622));
#31824=CARTESIAN_POINT('Ctrl Pts',(1.36229586747244,-2.6294307386282,1.71349583108653));
#31825=CARTESIAN_POINT('Ctrl Pts',(-1.43351324256106,-2.59128831836252,
1.55699563256684));
#31826=CARTESIAN_POINT('Ctrl Pts',(-2.95138608603967,-0.243085175943775,
1.40049543404715));
#31827=CARTESIAN_POINT('Ctrl Pts',(-1.83816183321196,2.32183838356734,1.24399523552746));
#31828=CARTESIAN_POINT('Ctrl Pts',(0.913719077918246,2.81687000661548,1.08749503700777));
#31829=CARTESIAN_POINT('Ctrl Pts',(2.85107841334811,0.800791217552173,0.930994838488081));
#31830=CARTESIAN_POINT('Ctrl Pts',(2.24670269063477,-1.92928650629548,0.774494639968393));
#31831=CARTESIAN_POINT('Ctrl Pts',(-0.360418976588814,-2.93923542656005,
0.617994441448702));
#31832=CARTESIAN_POINT('Ctrl Pts',(-2.64649260465595,-1.32934744147468,
0.461494242929014));
#31833=CARTESIAN_POINT('Ctrl Pts',(-2.57279134224077,1.46642423733366,0.304994044409324));
#31834=CARTESIAN_POINT('Ctrl Pts',(-0.206457409028375,2.95336916756547,
0.148493845889635));
#31835=CARTESIAN_POINT('Ctrl Pts',(2.34575618383328,1.81045825905282,-0.00800635263005447));
#31836=CARTESIAN_POINT('Ctrl Pts',(2.80318192056183,-0.952475183634134,
-0.164506551149743));
#31837=CARTESIAN_POINT('Ctrl Pts',(1.44737299166554,-2.21896863600185,-0.268840016829536));
#31838=CARTESIAN_POINT('Ctrl Pts',(0.650199997975074,-2.43208680203508,
-0.321006749669432));
#31839=CARTESIAN_POINT('Ctrl Pts',(2.05433155034209,1.75642532122685,5.10700224988981));
#31840=CARTESIAN_POINT('Ctrl Pts',(2.63004078503903,1.08307039382514,5.05483551704991));
#31841=CARTESIAN_POINT('Ctrl Pts',(3.05941317763178,-0.862009977081469,
4.95050205137012));
#31842=CARTESIAN_POINT('Ctrl Pts',(0.974440971474582,-3.02839279553707,
4.79400185285044));
#31843=CARTESIAN_POINT('Ctrl Pts',(-1.97873471034476,-2.48749909718309,
4.63750165433074));
#31844=CARTESIAN_POINT('Ctrl Pts',(-3.16812424993844,0.26717277658844,4.48100145581105));
#31845=CARTESIAN_POINT('Ctrl Pts',(-1.53310734151155,2.78561043396588,4.32450125729137));
#31846=CARTESIAN_POINT('Ctrl Pts',(1.46858378046875,2.81973520375758,4.16800105877167));
#31847=CARTESIAN_POINT('Ctrl Pts',(3.16109646255838,0.34066233277957,4.01150086025199));
#31848=CARTESIAN_POINT('Ctrl Pts',(2.03555600294299,-2.44237656098578,3.8550006617323));
#31849=CARTESIAN_POINT('Ctrl Pts',(-0.904624540810224,-3.0479547870335,
3.69850046321261));
#31850=CARTESIAN_POINT('Ctrl Pts',(-3.03835869183547,-0.936431501320334,
3.54200026469292));
#31851=CARTESIAN_POINT('Ctrl Pts',(-2.46346964861608,2.00993589020025,3.38550006617323));
#31852=CARTESIAN_POINT('Ctrl Pts',(0.307540244540666,3.16447528062537,3.22899986765354));
#31853=CARTESIAN_POINT('Ctrl Pts',(2.8043862016458,1.49797418738198,3.07249966913385));
#31854=CARTESIAN_POINT('Ctrl Pts',(2.80119136608943,-1.50393907013431,2.91599947061416));
#31855=CARTESIAN_POINT('Ctrl Pts',(0.300804243168747,-3.16512526420069,
2.75949927209447));
#31856=CARTESIAN_POINT('Ctrl Pts',(-2.46774239845802,-2.0046824284028,2.60299907357478));
#31857=CARTESIAN_POINT('Ctrl Pts',(-3.03635816138303,0.942885507987068,
2.44649887505509));
#31858=CARTESIAN_POINT('Ctrl Pts',(-0.898135981369886,3.04989441503522,
2.28999867653541));
#31859=CARTESIAN_POINT('Ctrl Pts',(2.04075168557006,2.43799788528061,2.13349847801572));
#31860=CARTESIAN_POINT('Ctrl Pts',(3.16036077240454,-0.347311941022739,
1.97699827949603));
#31861=CARTESIAN_POINT('Ctrl Pts',(1.46258537456475,-2.82300418989299,1.82049808097634));
#31862=CARTESIAN_POINT('Ctrl Pts',(-1.53904563089127,-2.78205380065442,
1.66399788245665));
#31863=CARTESIAN_POINT('Ctrl Pts',(-3.16866124841479,-0.260980622196635,
1.50749768393696));
#31864=CARTESIAN_POINT('Ctrl Pts',(-1.9734836444355,2.49276749859725,1.35099748541727));
#31865=CARTESIAN_POINT('Ctrl Pts',(0.98098525565046,3.02424236327596,1.19449728689758));
#31866=CARTESIAN_POINT('Ctrl Pts',(3.06096912474454,0.859743871237576,1.03799708837789));
#31867=CARTESIAN_POINT('Ctrl Pts',(2.41210046567521,-2.0713167343657,0.881496889858203));
#31868=CARTESIAN_POINT('Ctrl Pts',(-0.386952303432029,-3.15561608159711,
0.724996691338513));
#31869=CARTESIAN_POINT('Ctrl Pts',(-2.84132211649822,-1.42721135110194,
0.568496492818825));
#31870=CARTESIAN_POINT('Ctrl Pts',(-2.76219511400983,1.57437946751671,0.411996294299135));
#31871=CARTESIAN_POINT('Ctrl Pts',(-0.221656392069724,3.1707903204508,0.255496095779446));
#31872=CARTESIAN_POINT('Ctrl Pts',(2.51844607965735,1.94374058835217,0.0989958972597565));
#31873=CARTESIAN_POINT('Ctrl Pts',(3.00954658760352,-1.02259450863918,-0.0575043012599319));
#31874=CARTESIAN_POINT('Ctrl Pts',(1.55392570710626,-2.38232468520636,-0.161837766939725));
#31875=CARTESIAN_POINT('Ctrl Pts',(0.698066426160992,-2.61113218593862,
-0.214004499779622));
#31876=CARTESIAN_POINT('Ctrl Pts',(2.19519710401912,1.87686343907875,5.21400449977962));
#31877=CARTESIAN_POINT('Ctrl Pts',(2.81038273194434,1.15733655143342,5.16183776693973));
#31878=CARTESIAN_POINT('Ctrl Pts',(3.26919719770494,-0.921118017687907,
5.05750430125993));
#31879=CARTESIAN_POINT('Ctrl Pts',(1.04125840751576,-3.23604974741702,4.90100410274025));
#31880=CARTESIAN_POINT('Ctrl Pts',(-2.11441658725808,-2.65806695782732,
4.74450390422055));
#31881=CARTESIAN_POINT('Ctrl Pts',(-3.38536259031776,0.285492818986313,
4.58800370570087));
#31882=CARTESIAN_POINT('Ctrl Pts',(-1.63823254122548,2.97661979467193,4.43150350718118));
#31883=CARTESIAN_POINT('Ctrl Pts',(1.56928459836856,3.01308450058056,4.27500330866148));
#31884=CARTESIAN_POINT('Ctrl Pts',(3.37785290742272,0.364021555450283,4.1185031101418));
#31885=CARTESIAN_POINT('Ctrl Pts',(2.17513411697596,-2.60985036846042,3.96200291162211));
#31886=CARTESIAN_POINT('Ctrl Pts',(-0.966654662866148,-3.25695310504431,
3.80550271310242));
#31887=CARTESIAN_POINT('Ctrl Pts',(-3.24669900541512,-1.00064262726645,
3.64900251458273));
#31888=CARTESIAN_POINT('Ctrl Pts',(-2.63238980951274,2.1477572326127,3.49250231606304));
#31889=CARTESIAN_POINT('Ctrl Pts',(0.328628284987678,3.38146341110915,3.33600211754336));
#31890=CARTESIAN_POINT('Ctrl Pts',(2.99668301710058,1.60069030604565,3.17950191902366));
#31891=CARTESIAN_POINT('Ctrl Pts',(2.99326911160904,-1.60706420092233,3.02300172050398));
#31892=CARTESIAN_POINT('Ctrl Pts',(0.321430395872926,-3.38215796407065,
2.86650152198428));
#31893=CARTESIAN_POINT('Ctrl Pts',(-2.63695554189302,-2.14214354083938,
2.71000132346459));
#31894=CARTESIAN_POINT('Ctrl Pts',(-3.24456129855131,1.0075391852937,2.55350112494491));
#31895=CARTESIAN_POINT('Ctrl Pts',(-0.959721182780959,3.25902573337519,
2.39700092642522));
#31896=CARTESIAN_POINT('Ctrl Pts',(2.18068606766009,2.60517144687844,2.24050072790553));
#31897=CARTESIAN_POINT('Ctrl Pts',(3.37706677098096,-0.371127127457793,
2.08400052938584));
#31898=CARTESIAN_POINT('Ctrl Pts',(1.56287488165706,-3.01657764115777,1.92750033086615));
#31899=CARTESIAN_POINT('Ctrl Pts',(-1.64457801922149,-2.97281928294631,
1.77100013234646));
#31900=CARTESIAN_POINT('Ctrl Pts',(-3.3859364107899,-0.278876068449496,
1.61449993382677));
#31901=CARTESIAN_POINT('Ctrl Pts',(-2.10880545565905,2.66369661362717,1.45799973530708));
#31902=CARTESIAN_POINT('Ctrl Pts',(1.04825143338267,3.23161471993643,1.30149953678739));
#31903=CARTESIAN_POINT('Ctrl Pts',(3.27085983614097,0.918696524922978,1.1449993382677));
#31904=CARTESIAN_POINT('Ctrl Pts',(2.57749824071565,-2.21334696243591,0.988499139748014));
#31905=CARTESIAN_POINT('Ctrl Pts',(-0.413485630275245,-3.37199673663417,
0.831998941228324));
#31906=CARTESIAN_POINT('Ctrl Pts',(-3.03615162834048,-1.52507526072921,
0.675498742708636));
#31907=CARTESIAN_POINT('Ctrl Pts',(-2.9515988857789,1.68233469769977,0.518998544188945));
#31908=CARTESIAN_POINT('Ctrl Pts',(-0.23685537511107,3.38821147333612,0.362498345669257));
#31909=CARTESIAN_POINT('Ctrl Pts',(2.69113597548142,2.07702291765152,0.205998147149567));
#31910=CARTESIAN_POINT('Ctrl Pts',(3.21591125464521,-1.09271383364422,0.049497948629879));
#31911=CARTESIAN_POINT('Ctrl Pts',(1.66047842254699,-2.54568073441086,-0.0548355170499141));
#31912=CARTESIAN_POINT('Ctrl Pts',(0.745932854346909,-2.79017756984216,
-0.107002249889811));
#31913=CARTESIAN_POINT('Ctrl Pts',(2.33606265769615,1.99730155693065,5.32100674966943));
#31914=CARTESIAN_POINT('Ctrl Pts',(2.99072467884965,1.23160270904171,5.26884001682954));
#31915=CARTESIAN_POINT('Ctrl Pts',(3.47898121777811,-0.980226058294341,
5.16450655114975));
#31916=CARTESIAN_POINT('Ctrl Pts',(1.10807584355693,-3.44370669929698,5.00800635263005));
#31917=CARTESIAN_POINT('Ctrl Pts',(-2.25009846417141,-2.82863481847156,
4.85150615411037));
#31918=CARTESIAN_POINT('Ctrl Pts',(-3.60260093069709,0.30381286138419,4.69500595559067));
#31919=CARTESIAN_POINT('Ctrl Pts',(-1.74335774093941,3.16762915537798,4.53850575707099));
#31920=CARTESIAN_POINT('Ctrl Pts',(1.66998541626837,3.20643379740356,4.3820055585513));
#31921=CARTESIAN_POINT('Ctrl Pts',(3.59460935228705,0.387380778120988,4.22550536003161));
#31922=CARTESIAN_POINT('Ctrl Pts',(2.31471223100892,-2.77732417593505,4.06900516151192));
#31923=CARTESIAN_POINT('Ctrl Pts',(-1.02868478492208,-3.46595142305511,
3.91250496299223));
#31924=CARTESIAN_POINT('Ctrl Pts',(-3.45503931899475,-1.06485375321257,
3.75600476447254));
#31925=CARTESIAN_POINT('Ctrl Pts',(-2.8013099704094,2.28557857502515,3.59950456595285));
#31926=CARTESIAN_POINT('Ctrl Pts',(0.349716325434694,3.59845154159293,3.44300436743317));
#31927=CARTESIAN_POINT('Ctrl Pts',(3.18897983255535,1.70340642470933,3.28650416891347));
#31928=CARTESIAN_POINT('Ctrl Pts',(3.18534685712864,-1.71018933171035,3.13000397039378));
#31929=CARTESIAN_POINT('Ctrl Pts',(0.342056548577105,-3.59919066394061,
2.9735037718741));
#31930=CARTESIAN_POINT('Ctrl Pts',(-2.80616868532801,-2.27960465327595,
2.8170035733544));
#31931=CARTESIAN_POINT('Ctrl Pts',(-3.45276443571958,1.07219286260033,2.66050337483472));
#31932=CARTESIAN_POINT('Ctrl Pts',(-1.02130638419203,3.46815705171515,2.50400317631503));
#31933=CARTESIAN_POINT('Ctrl Pts',(2.32062044975012,2.77234500847627,2.34750297779534));
#31934=CARTESIAN_POINT('Ctrl Pts',(3.59377276955738,-0.394942313892847,
2.19100277927565));
#31935=CARTESIAN_POINT('Ctrl Pts',(1.66316438874938,-3.21015109242256,2.03450258075596));
#31936=CARTESIAN_POINT('Ctrl Pts',(-1.7501104075517,-3.16358476523821,1.87800238223627));
#31937=CARTESIAN_POINT('Ctrl Pts',(-3.60321157316502,-0.296771514702359,
1.72150218371658));
#31938=CARTESIAN_POINT('Ctrl Pts',(-2.2441272668826,2.83462572865708,1.56500198519689));
#31939=CARTESIAN_POINT('Ctrl Pts',(1.11551761111489,3.4389870765969,1.4085017866772));
#31940=CARTESIAN_POINT('Ctrl Pts',(3.48075054753741,0.977649178608381,1.25200158815752));
#31941=CARTESIAN_POINT('Ctrl Pts',(2.74289601575609,-2.35537719050612,1.09550138963782));
#31942=CARTESIAN_POINT('Ctrl Pts',(-0.440018957118456,-3.58837739167123,
0.939001191118136));
#31943=CARTESIAN_POINT('Ctrl Pts',(-3.23098114018275,-1.62293917035647,
0.782500992598446));
#31944=CARTESIAN_POINT('Ctrl Pts',(-3.14100265754796,1.79028992788282,0.626000794078757));
#31945=CARTESIAN_POINT('Ctrl Pts',(-0.25205435815242,3.60563262622145,0.469500595559067));
#31946=CARTESIAN_POINT('Ctrl Pts',(2.8638258713055,2.21030524695087,0.313000397039378));
#31947=CARTESIAN_POINT('Ctrl Pts',(3.4222759216869,-1.16283315864926,0.15650019851969));
#31948=CARTESIAN_POINT('Ctrl Pts',(1.76703113798771,-2.70903678361537,0.0521667328398966));
#31949=CARTESIAN_POINT('Ctrl Pts',(0.793799282532827,-2.96922295374571,
0.));
#31950=CARTESIAN_POINT('Ctrl Pts',(0.793799282532827,-2.96922295374571,
0.));
#31951=CARTESIAN_POINT('Ctrl Pts',(0.886893769048896,-2.93516857472777,
6.49317190359092E-17));
#31952=CARTESIAN_POINT('Ctrl Pts',(0.977926242508662,-2.8963539026744,3.5899553935387E-16));
#31953=CARTESIAN_POINT('Ctrl Pts',(1.06668623690149,-2.85310458823344,2.77555756156289E-16));
#31954=CARTESIAN_POINT('Ctrl Pts',(1.1573833631875,-2.8089113842966,1.94338600140189E-16));
#31955=CARTESIAN_POINT('Ctrl Pts',(1.24570840723307,-2.76008724482105,8.94098625496742E-16));
#31956=CARTESIAN_POINT('Ctrl Pts',(1.33140791312673,-2.70693413976456,1.38777878078145E-15));
#31957=CARTESIAN_POINT('Ctrl Pts',(1.41293443628286,-2.65636922920854,1.85742007207992E-15));
#31958=CARTESIAN_POINT('Ctrl Pts',(1.49208510125195,-2.60188577643099,1.19996770961849E-15));
#31959=CARTESIAN_POINT('Ctrl Pts',(1.5686100025003,-2.54371483646266,1.16573417585641E-15));
#31960=CARTESIAN_POINT('Ctrl Pts',(1.63556929109261,-2.49281526399038,1.1357798338146E-15));
#31961=CARTESIAN_POINT('Ctrl Pts',(1.70051795047849,-2.43909179704035,4.6524848618713E-16));
#31962=CARTESIAN_POINT('Ctrl Pts',(1.7632650317936,-2.38268698713509,5.55111512312578E-16));
#31963=CARTESIAN_POINT('Ctrl Pts',(1.77895111395862,-2.36858640326518,5.7757628329248E-16));
#31964=CARTESIAN_POINT('Ctrl Pts',(1.79450367669767,-2.35431414158982,1.61759689860544E-15));
#31965=CARTESIAN_POINT('Ctrl Pts',(1.80989558143071,-2.33989519409729,1.66533453693773E-15));
#31966=CARTESIAN_POINT('Ctrl Pts',(1.88231905248557,-2.27204977506178,1.88995426581157E-15));
#31967=CARTESIAN_POINT('Ctrl Pts',(1.95127638915324,-2.2008843069976,9.33280417709878E-16));
#31968=CARTESIAN_POINT('Ctrl Pts',(2.01652605934852,-2.12668615788006,7.49400541621981E-16));
#31969=CARTESIAN_POINT('Ctrl Pts',(2.08140793958276,-2.05290623822316,5.66557133186095E-16));
#31970=CARTESIAN_POINT('Ctrl Pts',(2.14262432088329,-1.97612693884884,9.5775323130718E-16));
#31971=CARTESIAN_POINT('Ctrl Pts',(2.19989413197892,-1.89660402190249,6.93889390390723E-16));
#31972=CARTESIAN_POINT('Ctrl Pts',(2.25380415733742,-1.82174638945804,4.45505362525734E-16));
#31973=CARTESIAN_POINT('Ctrl Pts',(2.30421707668655,-1.74445688295852,3.26466360005673E-15));
#31974=CARTESIAN_POINT('Ctrl Pts',(2.35085702030783,-1.6649361419825,3.7470027081099E-15));
#31975=CARTESIAN_POINT('Ctrl Pts',(2.38695907926369,-1.60338241236736,4.12036154098178E-15));
#31976=CARTESIAN_POINT('Ctrl Pts',(2.42079974187715,-1.54049148436203,2.76023327184715E-15));
#31977=CARTESIAN_POINT('Ctrl Pts',(2.45223230030139,-1.47635450699168,2.80331313717852E-15));
#31978=CARTESIAN_POINT('Ctrl Pts',(2.45885027647649,-1.46285077043765,2.81238339861069E-15));
#31979=CARTESIAN_POINT('Ctrl Pts',(2.46536173765269,-1.4492909927482,2.25462528933555E-15));
#31980=CARTESIAN_POINT('Ctrl Pts',(2.47175843746063,-1.43569095783397,2.27595720048157E-15));
#31981=CARTESIAN_POINT('Ctrl Pts',(2.51224387039329,-1.34961480639136,2.41096926669652E-15));
#31982=CARTESIAN_POINT('Ctrl Pts',(2.5482055573203,-1.26178852463594,3.62029001511052E-15));
#31983=CARTESIAN_POINT('Ctrl Pts',(2.57938539343216,-1.17245068676435,3.44169137633799E-15));
#31984=CARTESIAN_POINT('Ctrl Pts',(2.61056522954403,-1.08311284889276,3.26309273756545E-15));
#31985=CARTESIAN_POINT('Ctrl Pts',(2.6369636677978,-0.99226274488999,1.94109001754332E-16));
#31986=CARTESIAN_POINT('Ctrl Pts',(2.65826790515113,-0.90012905980095,-3.60822483003176E-16));
#31987=CARTESIAN_POINT('Ctrl Pts',(2.67972711543533,-0.807325168734929,
-9.19790693281215E-16));
#31988=CARTESIAN_POINT('Ctrl Pts',(2.6960170532411,-0.713217781371016,2.19518166871644E-16));
#31989=CARTESIAN_POINT('Ctrl Pts',(2.70721235053312,-0.618215105888531,
0.));
#31990=CARTESIAN_POINT('Ctrl Pts',(2.71292160521868,-0.56976668544991,-1.11947462410922E-16));
#31991=CARTESIAN_POINT('Ctrl Pts',(2.71730508064361,-0.521085594130936,
7.31925815782227E-16));
#31992=CARTESIAN_POINT('Ctrl Pts',(2.72036776812806,-0.472227710003176,
7.49400541621981E-16));
#31993=CARTESIAN_POINT('Ctrl Pts',(2.72142942533794,-0.455291497866967,
7.55458021783632E-16));
#31994=CARTESIAN_POINT('Ctrl Pts',(2.72233234751915,-0.438334056241388,
1.47771822505628E-15));
#31995=CARTESIAN_POINT('Ctrl Pts',(2.72307665503345,-0.421357761541496,
1.52655665885959E-15));
#31996=CARTESIAN_POINT('Ctrl Pts',(2.72371406196817,-0.40681967377542,1.56838071113613E-15));
#31997=CARTESIAN_POINT('Ctrl Pts',(2.72423475300693,-0.392276144899293,
-5.84163957766239E-16));
#31998=CARTESIAN_POINT('Ctrl Pts',(2.72463912967391,-0.377733018449256,
-5.82867087928207E-16));
#31999=CARTESIAN_POINT('Ctrl Pts',(2.7272335888012,-0.284425094826578,-5.74546440218005E-16));
#32000=CARTESIAN_POINT('Ctrl Pts',(2.72504700910767,-0.191075061278942,
2.51838167646803E-15));
#32001=CARTESIAN_POINT('Ctrl Pts',(2.71820565462271,-0.0980605230163078,
1.9151347174784E-15));
#32002=CARTESIAN_POINT('Ctrl Pts',(2.71136113957177,-0.00500301393752514,
1.31160907071961E-15));
#32003=CARTESIAN_POINT('Ctrl Pts',(2.69985717427859,0.0877196672682859,
-3.07238256336187E-16));
#32004=CARTESIAN_POINT('Ctrl Pts',(2.68376968445062,0.179716676654276,-1.04083408558608E-15));
#32005=CARTESIAN_POINT('Ctrl Pts',(2.6679263547778,0.270317445587206,-1.76329611625024E-15));
#32006=CARTESIAN_POINT('Ctrl Pts',(2.64763712143603,0.360215237891958,2.87404250511705E-16));
#32007=CARTESIAN_POINT('Ctrl Pts',(2.62293183221363,0.449011051883673,-1.38777878078145E-17));
#32008=CARTESIAN_POINT('Ctrl Pts',(2.6135041541326,0.482896036662513,-1.28848717445863E-16));
#32009=CARTESIAN_POINT('Ctrl Pts',(2.60343298467484,0.516620214186245,-4.06891175216909E-16));
#32010=CARTESIAN_POINT('Ctrl Pts',(2.592718513,0.550160020505481,-5.82867087928207E-16));
#32011=CARTESIAN_POINT('Ctrl Pts',(2.58640686113371,0.569917558494655,-6.86530500515623E-16));
#32012=CARTESIAN_POINT('Ctrl Pts',(2.57987196088238,0.589611101451674,-5.51406606223906E-16));
#32013=CARTESIAN_POINT('Ctrl Pts',(2.57311372784884,0.609235684372638,-7.21644966006352E-16));
#32014=CARTESIAN_POINT('Ctrl Pts',(2.56765136113167,0.625097325729763,-8.59240746715142E-16));
#32015=CARTESIAN_POINT('Ctrl Pts',(2.56204545311482,0.640906940190805,1.0191622183722E-15));
#32016=CARTESIAN_POINT('Ctrl Pts',(2.55629874325467,0.656655644997032,1.08246744900953E-15));
#32017=CARTESIAN_POINT('Ctrl Pts',(2.52550685343402,0.741039996219253,1.42166809325501E-15));
#32018=CARTESIAN_POINT('Ctrl Pts',(2.49065541114871,0.823737254187918,2.9255481979655E-15));
#32019=CARTESIAN_POINT('Ctrl Pts',(2.45179432548469,0.904376871334311,3.03229663600746E-15));
#32020=CARTESIAN_POINT('Ctrl Pts',(2.42326928916242,0.96356842424157,3.11065273492912E-15));
#32021=CARTESIAN_POINT('Ctrl Pts',(2.39258299461189,1.0216508685957,2.15271533017043E-15));
#32022=CARTESIAN_POINT('Ctrl Pts',(2.35974245541383,1.07846525592557,2.35922392732846E-15));
#32023=CARTESIAN_POINT('Ctrl Pts',(2.3470744452395,1.1003810117054,2.43888318609111E-15));
#32024=CARTESIAN_POINT('Ctrl Pts',(2.33408578165144,1.12210795602091,1.70584578534577E-15));
#32025=CARTESIAN_POINT('Ctrl Pts',(2.32077647825335,1.14363645354687,1.81799020282369E-15));
#32026=CARTESIAN_POINT('Ctrl Pts',(2.30811732205646,1.16411330381573,1.92465646889336E-15));
#32027=CARTESIAN_POINT('Ctrl Pts',(2.29516525813278,1.18441464884107,-2.41812693860714E-17));
#32028=CARTESIAN_POINT('Ctrl Pts',(2.28193698658913,1.20450712017389,0.));
#32029=CARTESIAN_POINT('Ctrl Pts',(2.23464326966583,1.27634172444316,8.6452875223902E-17));
#32030=CARTESIAN_POINT('Ctrl Pts',(2.18378846776941,1.34556635950281,1.71218066021624E-15));
#32031=CARTESIAN_POINT('Ctrl Pts',(2.1293995805356,1.4118263229903,7.73686670285656E-16));
#32032=CARTESIAN_POINT('Ctrl Pts',(2.09060596956493,1.45908713999166,1.04293112238207E-16));
#32033=CARTESIAN_POINT('Ctrl Pts',(2.05001367990221,1.50483902366414,-3.15793211228134E-16));
#32034=CARTESIAN_POINT('Ctrl Pts',(2.00762309288065,1.54893995061572,-2.67147415300428E-16));
#32035=CARTESIAN_POINT('Ctrl Pts',(1.9782489136182,1.57949929468088,-2.39592455248551E-16));
#32036=CARTESIAN_POINT('Ctrl Pts',(1.94801102665337,1.60926561951879,-8.19373708274163E-16));
#32037=CARTESIAN_POINT('Ctrl Pts',(1.91694983752522,1.63822102714876,-8.32667268468867E-16));
#32038=CARTESIAN_POINT('Ctrl Pts',(1.91346599666506,1.63598720337495,5.));
#32039=CARTESIAN_POINT('Ctrl Pts',(1.97511426248036,1.57805297138613,5.));
#32040=CARTESIAN_POINT('Ctrl Pts',(2.0333992327661,1.51697077668011,5.));
#32041=CARTESIAN_POINT('Ctrl Pts',(2.08832045660242,1.45312471107507,5.));
#32042=CARTESIAN_POINT('Ctrl Pts',(2.14469107178614,1.38759372425762,5.));
#32043=CARTESIAN_POINT('Ctrl Pts',(2.19751849836391,1.31915063045882,5.));
#32044=CARTESIAN_POINT('Ctrl Pts',(2.2467768545975,1.24816218982756,5.));
#32045=CARTESIAN_POINT('Ctrl Pts',(2.29674569779122,1.17614983436752,5.));
#32046=CARTESIAN_POINT('Ctrl Pts',(2.34304221736815,1.10151755915666,5.));
#32047=CARTESIAN_POINT('Ctrl Pts',(2.38560686750513,1.02460707565943,5.));
#32048=CARTESIAN_POINT('Ctrl Pts',(2.40516281592033,0.989271240805406,5.));
#32049=CARTESIAN_POINT('Ctrl Pts',(2.42393052938809,0.953453999419588,5.));
#32050=CARTESIAN_POINT('Ctrl Pts',(2.44190157522008,0.917186211225675,5.));
#32051=CARTESIAN_POINT('Ctrl Pts',(2.45212589418763,0.896552273823891,5.));
#32052=CARTESIAN_POINT('Ctrl Pts',(2.46209231213777,0.875772477886718,5.));
#32053=CARTESIAN_POINT('Ctrl Pts',(2.47179901297218,0.854852339979442,5.));
#32054=CARTESIAN_POINT('Ctrl Pts',(2.47986584870041,0.837466482643475,5.));
#32055=CARTESIAN_POINT('Ctrl Pts',(2.48775529546885,0.819978882487774,5.));
#32056=CARTESIAN_POINT('Ctrl Pts',(2.49545397654565,0.802421362463391,5.));
#32057=CARTESIAN_POINT('Ctrl Pts',(2.53207516621785,0.718903515111055,5.));
#32058=CARTESIAN_POINT('Ctrl Pts',(2.56443375074574,0.633702408588491,5.));
#32059=CARTESIAN_POINT('Ctrl Pts',(2.59250161927242,0.547215516795963,5.));
#32060=CARTESIAN_POINT('Ctrl Pts',(2.62102734916793,0.459317794443813,5.));
#32061=CARTESIAN_POINT('Ctrl Pts',(2.64512173324747,0.370091241926015,5.));
#32062=CARTESIAN_POINT('Ctrl Pts',(2.6647162612932,0.279916019321374,5.));
#32063=CARTESIAN_POINT('Ctrl Pts',(2.68327377745922,0.194513189135613,5.));
#32064=CARTESIAN_POINT('Ctrl Pts',(2.69779512543597,0.108258519972062,5.));
#32065=CARTESIAN_POINT('Ctrl Pts',(2.70818462605886,0.0214547457753918,
5.));
#32066=CARTESIAN_POINT('Ctrl Pts',(2.71280315092634,-0.0171328056643356,
5.));
#32067=CARTESIAN_POINT('Ctrl Pts',(2.71660465425308,-0.0558290637111655,
5.));
#32068=CARTESIAN_POINT('Ctrl Pts',(2.71957815680565,-0.0946081258455055,
5.));
#32069=CARTESIAN_POINT('Ctrl Pts',(2.72114193269849,-0.115002176780577,
5.));
#32070=CARTESIAN_POINT('Ctrl Pts',(2.72247667707736,-0.135419134083706,
5.));
#32071=CARTESIAN_POINT('Ctrl Pts',(2.72358060529281,-0.155855252406095,
5.));
#32072=CARTESIAN_POINT('Ctrl Pts',(2.72440760299952,-0.171164783180025,
5.));
#32073=CARTESIAN_POINT('Ctrl Pts',(2.72510503301269,-0.186486473786052,
5.));
#32074=CARTESIAN_POINT('Ctrl Pts',(2.72567165779787,-0.201800403224458,
5.));
#32075=CARTESIAN_POINT('Ctrl Pts',(2.72919576912562,-0.297045075921046,
5.));
#32076=CARTESIAN_POINT('Ctrl Pts',(2.72767362176579,-0.39214594976183,5.));
#32077=CARTESIAN_POINT('Ctrl Pts',(2.72104232884131,-0.48670474660219,5.));
#32078=CARTESIAN_POINT('Ctrl Pts',(2.71460574319996,-0.578487118597797,
5.));
#32079=CARTESIAN_POINT('Ctrl Pts',(2.70335577583384,-0.669759723511558,
5.));
#32080=CARTESIAN_POINT('Ctrl Pts',(2.68719094334706,-0.76017485193479,5.));
#32081=CARTESIAN_POINT('Ctrl Pts',(2.67098570391041,-0.850815989477801,
5.));
#32082=CARTESIAN_POINT('Ctrl Pts',(2.64984154989292,-0.940596245438192,
5.));
#32083=CARTESIAN_POINT('Ctrl Pts',(2.62403295621111,-1.02927270988445,5.));
#32084=CARTESIAN_POINT('Ctrl Pts',(2.60893641023223,-1.08114335185981,5.));
#32085=CARTESIAN_POINT('Ctrl Pts',(2.59224287435959,-1.13263631317645,5.));
#32086=CARTESIAN_POINT('Ctrl Pts',(2.57399925344803,-1.18370190437231,5.));
#32087=CARTESIAN_POINT('Ctrl Pts',(2.56913720383633,-1.19731123330153,5.));
#32088=CARTESIAN_POINT('Ctrl Pts',(2.5641650271584,-1.21089020050661,5.));
#32089=CARTESIAN_POINT('Ctrl Pts',(2.55908354497344,-1.22443784743359,5.));
#32090=CARTESIAN_POINT('Ctrl Pts',(2.55395835978812,-1.23810201013234,5.));
#32091=CARTESIAN_POINT('Ctrl Pts',(2.5487251194683,-1.25172589600239,5.));
#32092=CARTESIAN_POINT('Ctrl Pts',(2.54338628977321,-1.26530561093663,5.));
#32093=CARTESIAN_POINT('Ctrl Pts',(2.507474434899,-1.35665011521995,5.));
#32094=CARTESIAN_POINT('Ctrl Pts',(2.46677381849346,-1.44603954020521,5.));
#32095=CARTESIAN_POINT('Ctrl Pts',(2.42165814194307,-1.53319842974304,5.));
#32096=CARTESIAN_POINT('Ctrl Pts',(2.37698904164233,-1.61949457947533,5.));
#32097=CARTESIAN_POINT('Ctrl Pts',(2.32799127252537,-1.70360490076703,5.));
#32098=CARTESIAN_POINT('Ctrl Pts',(2.27497065048649,-1.78525830139829,5.));
#32099=CARTESIAN_POINT('Ctrl Pts',(2.22143189817264,-1.86770963870577,5.));
#32100=CARTESIAN_POINT('Ctrl Pts',(2.16379086711139,-1.94765663398949,5.));
#32101=CARTESIAN_POINT('Ctrl Pts',(2.10231135200038,-2.02480429723545,5.));
#32102=CARTESIAN_POINT('Ctrl Pts',(2.07897018428145,-2.05409399712484,5.));
#32103=CARTESIAN_POINT('Ctrl Pts',(2.05507524958568,-2.08297997370897,5.));
#32104=CARTESIAN_POINT('Ctrl Pts',(2.03063928040512,-2.11144510112202,5.));
#32105=CARTESIAN_POINT('Ctrl Pts',(2.01356866368511,-2.13133042985048,5.));
#32106=CARTESIAN_POINT('Ctrl Pts',(1.99623399133744,-2.1510103628177,5.));
#32107=CARTESIAN_POINT('Ctrl Pts',(1.97863935752325,-2.17047886391133,5.));
#32108=CARTESIAN_POINT('Ctrl Pts',(1.96848269337448,-2.18171723517703,5.));
#32109=CARTESIAN_POINT('Ctrl Pts',(1.95824201635888,-2.19288219327417,5.));
#32110=CARTESIAN_POINT('Ctrl Pts',(1.94792378478368,-2.20396685638102,5.));
#32111=CARTESIAN_POINT('Ctrl Pts',(1.87693652902952,-2.28022699933091,5.));
#32112=CARTESIAN_POINT('Ctrl Pts',(1.80220735563424,-2.35277244990143,5.));
#32113=CARTESIAN_POINT('Ctrl Pts',(1.7240709087608,-2.42127737465979,5.));
#32114=CARTESIAN_POINT('Ctrl Pts',(1.66546857360572,-2.47265606822857,5.));
#32115=CARTESIAN_POINT('Ctrl Pts',(1.60494837513541,-2.52176172516572,5.));
#32116=CARTESIAN_POINT('Ctrl Pts',(1.5426329601745,-2.56844590489654,5.));
#32117=CARTESIAN_POINT('Ctrl Pts',(1.50966649198766,-2.5931430448721,5.));
#32118=CARTESIAN_POINT('Ctrl Pts',(1.47619735041169,-2.61716230488521,5.));
#32119=CARTESIAN_POINT('Ctrl Pts',(1.44224214591351,-2.64048025951079,5.));
#32120=CARTESIAN_POINT('Ctrl Pts',(1.42523499995595,-2.65215952528491,5.));
#32121=CARTESIAN_POINT('Ctrl Pts',(1.40811304383442,-2.66365787868399,5.));
#32122=CARTESIAN_POINT('Ctrl Pts',(1.39088369966999,-2.6749695061669,5.));
#32123=CARTESIAN_POINT('Ctrl Pts',(1.30563891492228,-2.73093549307415,5.));
#32124=CARTESIAN_POINT('Ctrl Pts',(1.2177306352799,-2.78235921066159,5.));
#32125=CARTESIAN_POINT('Ctrl Pts',(1.12744207813993,-2.82892525415745,5.));
#32126=CARTESIAN_POINT('Ctrl Pts',(1.06580281768531,-2.86071551168622,5.));
#32127=CARTESIAN_POINT('Ctrl Pts',(1.00305327491768,-2.89024121467184,5.));
#32128=CARTESIAN_POINT('Ctrl Pts',(0.939273877630842,-2.91739189131414,
5.));
#32129=CARTESIAN_POINT('Ctrl Pts',(0.891985416295931,-2.93752243153926,
5.));
#32130=CARTESIAN_POINT('Ctrl Pts',(0.84413064869809,-2.95634718738556,5.));
#32131=CARTESIAN_POINT('Ctrl Pts',(0.795759619474682,-2.97387964574988,
5.));
#32132=CARTESIAN_POINT('Ctrl Pts',(-2.51589013302272,-0.00197902614912163,
3.38741669750803));
#32133=CARTESIAN_POINT('Ctrl Pts',(-2.51781607531079,-0.253199548871946,
3.40327713660639));
#32134=CARTESIAN_POINT('Ctrl Pts',(-2.48311008876547,-0.503899930938732,
3.41913757570475));
#32135=CARTESIAN_POINT('Ctrl Pts',(-2.40953623658284,-0.742620570455294,
3.43499801480311));
#32136=CARTESIAN_POINT('Ctrl Pts',(-2.16754372508865,-1.52779907325704,
3.48716474764301));
#32137=CARTESIAN_POINT('Ctrl Pts',(-1.50506907192147,-2.18337777113987,
3.5393314804829));
#32138=CARTESIAN_POINT('Ctrl Pts',(-0.717403027393835,-2.41715816749602,
3.5914982133228));
#32139=CARTESIAN_POINT('Ctrl Pts',(0.0702630171338087,-2.65093856385218,
3.64366494616269));
#32140=CARTESIAN_POINT('Ctrl Pts',(0.983120453021916,-2.46292065868166,
3.69583167900259));
#32141=CARTESIAN_POINT('Ctrl Pts',(1.61427619242997,-1.93687739549307,3.74799841184249));
#32142=CARTESIAN_POINT('Ctrl Pts',(2.24543193183803,-1.41083413230447,3.80016514468238));
#32143=CARTESIAN_POINT('Ctrl Pts',(2.59488597476604,-0.546765511097805,
3.85233187752228));
#32144=CARTESIAN_POINT('Ctrl Pts',(2.50687015370919,0.270115932309816,3.90449861036218));
#32145=CARTESIAN_POINT('Ctrl Pts',(2.41885433265234,1.08699737571744,3.95666534320207));
#32146=CARTESIAN_POINT('Ctrl Pts',(1.89336864761064,1.85669164132601,4.00883207604197));
#32147=CARTESIAN_POINT('Ctrl Pts',(1.16464828769536,2.23624130185117,4.06099880888186));
#32148=CARTESIAN_POINT('Ctrl Pts',(0.435927927780085,2.61579096237633,4.11316554172176));
#32149=CARTESIAN_POINT('Ctrl Pts',(-0.496027107008767,2.60519601781808,
4.16533227456166));
#32150=CARTESIAN_POINT('Ctrl Pts',(-1.21582191903011,2.20894048902741,4.21749900740156));
#32151=CARTESIAN_POINT('Ctrl Pts',(-1.93561673105145,1.81268496023674,4.26966574024145));
#32152=CARTESIAN_POINT('Ctrl Pts',(-2.44325132030528,1.03076884721365,4.32183247308135));
#32153=CARTESIAN_POINT('Ctrl Pts',(-2.51242976891092,0.212180128913875,
4.37399920592124));
#32154=CARTESIAN_POINT('Ctrl Pts',(-2.51836075980379,0.141998702022978,
4.37847170311684));
#32155=CARTESIAN_POINT('Ctrl Pts',(-2.52106890854963,0.0715477156323498,
4.38294420031243));
#32156=CARTESIAN_POINT('Ctrl Pts',(-2.52065797473119,0.00106685237120291,
4.38741669750802));
#32157=CARTESIAN_POINT('Ctrl Pts',(-0.793799282532885,-2.96922295374569,
5.));
#32158=CARTESIAN_POINT('Ctrl Pts',(-1.76703113798775,-2.70903678361534,
4.9478332671601));
#32159=CARTESIAN_POINT('Ctrl Pts',(-3.42227762319113,-1.16284338723151,
4.84349980148031));
#32160=CARTESIAN_POINT('Ctrl Pts',(-2.86382437134345,2.21031103269041,4.68699960296062));
#32161=CARTESIAN_POINT('Ctrl Pts',(0.252054090990421,3.60562829022214,4.53049940444094));
#32162=CARTESIAN_POINT('Ctrl Pts',(3.14100203598835,1.79029184281612,4.37399920592124));
#32163=CARTESIAN_POINT('Ctrl Pts',(3.23098071080095,-1.62294021205589,4.21749900740156));
#32164=CARTESIAN_POINT('Ctrl Pts',(0.440018754334274,-3.58837598279832,
4.06099880888186));
#32165=CARTESIAN_POINT('Ctrl Pts',(-2.74289544065113,-2.35537722830823,
3.90449861036218));
#32166=CARTESIAN_POINT('Ctrl Pts',(-3.48074999950888,0.977649265989379,
3.74799841184248));
#32167=CARTESIAN_POINT('Ctrl Pts',(-1.11551737463701,3.43898632522653,3.5914982133228));
#32168=CARTESIAN_POINT('Ctrl Pts',(2.24412684766706,2.83462531411003,3.43499801480311));
#32169=CARTESIAN_POINT('Ctrl Pts',(3.60321095550619,-0.296771509319279,
3.27849781628342));
#32170=CARTESIAN_POINT('Ctrl Pts',(1.75011009124083,-3.16358418358746,3.12199761776373));
#32171=CARTESIAN_POINT('Ctrl Pts',(-1.66316409145381,-3.2101505430571,2.96549741924404));
#32172=CARTESIAN_POINT('Ctrl Pts',(-3.59377214139091,-0.394942236718185,
2.80899722072435));
#32173=CARTESIAN_POINT('Ctrl Pts',(-2.3206200405613,2.77234451758071,2.65249702220466));
#32174=CARTESIAN_POINT('Ctrl Pts',(1.02130620401276,3.46815644429995,2.49599682368497));
#32175=CARTESIAN_POINT('Ctrl Pts',(3.45276382958855,1.07219267437738,2.33949662516528));
#32176=CARTESIAN_POINT('Ctrl Pts',(2.8061681927767,-2.27960425476498,2.18299642664559));
#32177=CARTESIAN_POINT('Ctrl Pts',(-0.34205648942751,-3.59919002761108,
2.02649622812591));
#32178=CARTESIAN_POINT('Ctrl Pts',(-3.18534629574052,-1.71018903949051,
1.86999602960622));
#32179=CARTESIAN_POINT('Ctrl Pts',(-3.18897927637007,1.7034061403768,1.71349583108653));
#32180=CARTESIAN_POINT('Ctrl Pts',(-0.349716256635896,3.59845088308181,
1.55699563256684));
#32181=CARTESIAN_POINT('Ctrl Pts',(2.8013094644448,2.28557822072128,1.40049543404715));
#32182=CARTESIAN_POINT('Ctrl Pts',(3.45503873870173,-1.0648536490447,1.24399523552746));
#32183=CARTESIAN_POINT('Ctrl Pts',(1.02868455419652,-3.46595066989846,1.08749503700777));
#32184=CARTESIAN_POINT('Ctrl Pts',(-2.31471172988138,-2.77732393751975,
0.930994838488083));
#32185=CARTESIAN_POINT('Ctrl Pts',(-3.5946088997546,0.387381135037168,0.774494639968393));
#32186=CARTESIAN_POINT('Ctrl Pts',(-1.66998478533906,3.20643252148329,0.617994441448703));
#32187=CARTESIAN_POINT('Ctrl Pts',(1.74335679702331,3.1676297706248,0.461494242929015));
#32188=CARTESIAN_POINT('Ctrl Pts',(3.60260150316633,0.3038109312067,0.304994044409326));
#32189=CARTESIAN_POINT('Ctrl Pts',(2.25009578791265,-2.82863139649778,0.148493845889636));
#32190=CARTESIAN_POINT('Ctrl Pts',(-1.10807133015233,-3.44371061769541,
-0.00800635263005217));
#32191=CARTESIAN_POINT('Ctrl Pts',(-3.47898841388462,-0.980218592702346,
-0.164506551149742));
#32192=CARTESIAN_POINT('Ctrl Pts',(-2.99072467884965,1.23160270904172,-0.268840016829535));
#32193=CARTESIAN_POINT('Ctrl Pts',(-2.33606265769614,1.99730155693066,-0.321006749669431));
#32194=CARTESIAN_POINT('Ctrl Pts',(-0.745932854346964,-2.79017756984215,
5.10700224988981));
#32195=CARTESIAN_POINT('Ctrl Pts',(-1.66047842254703,-2.54568073441083,
5.05483551704991));
#32196=CARTESIAN_POINT('Ctrl Pts',(-3.21591285354802,-1.09272344543869,
4.95050205137012));
#32197=CARTESIAN_POINT('Ctrl Pts',(-2.69113456596771,2.07702835450855,4.79400185285043));
#32198=CARTESIAN_POINT('Ctrl Pts',(0.236855124059054,3.38820739879938,4.63750165433075));
#32199=CARTESIAN_POINT('Ctrl Pts',(2.95159830169959,1.68233649716179,4.48100145581105));
#32200=CARTESIAN_POINT('Ctrl Pts',(3.03615122485059,-1.52507623961371,4.32450125729137));
#32201=CARTESIAN_POINT('Ctrl Pts',(0.413485439719026,-3.37199541271688,
4.16800105877167));
#32202=CARTESIAN_POINT('Ctrl Pts',(-2.57749770028975,-2.21334699795853,
4.01150086025199));
#32203=CARTESIAN_POINT('Ctrl Pts',(-3.2708593211588,0.918696607034865,3.85500066173229));
#32204=CARTESIAN_POINT('Ctrl Pts',(-1.04825121116451,3.231614013874,3.69850046321261));
#32205=CARTESIAN_POINT('Ctrl Pts',(2.10880506172238,2.66369622407748,3.54200026469292));
#32206=CARTESIAN_POINT('Ctrl Pts',(3.38593583037616,-0.278876063391019,
3.38550006617323));
#32207=CARTESIAN_POINT('Ctrl Pts',(1.64457772198429,-2.97281873636934,3.22899986765354));
#32208=CARTESIAN_POINT('Ctrl Pts',(-1.56287460228854,-3.01657712491928,
3.07249966913385));
#32209=CARTESIAN_POINT('Ctrl Pts',(-3.37706618069319,-0.371127054936794,
2.91599947061416));
#32210=CARTESIAN_POINT('Ctrl Pts',(-2.18068568314553,2.60517098558408,2.75949927209447));
#32211=CARTESIAN_POINT('Ctrl Pts',(0.95972101346657,3.25902516258738,2.60299907357479));
#32212=CARTESIAN_POINT('Ctrl Pts',(3.24456072897023,1.00753900842068,2.44649887505509));
#32213=CARTESIAN_POINT('Ctrl Pts',(2.63695507904276,-2.14214316635878,2.28999867653541));
#32214=CARTESIAN_POINT('Ctrl Pts',(-0.321430340290076,-3.38215736611206,
2.13349847801571));
#32215=CARTESIAN_POINT('Ctrl Pts',(-2.99326858407285,-1.60706392632346,
1.97699827949603));
#32216=CARTESIAN_POINT('Ctrl Pts',(-2.9966824944535,1.60069003885849,1.82049808097634));
#32217=CARTESIAN_POINT('Ctrl Pts',(-0.32862822033748,3.38146279230653,1.66399788245665));
#32218=CARTESIAN_POINT('Ctrl Pts',(2.63238933405802,2.1477568996735,1.50749768393696));
#32219=CARTESIAN_POINT('Ctrl Pts',(3.246698460114,-1.00064252937995,1.35099748541727));
#32220=CARTESIAN_POINT('Ctrl Pts',(0.96665444605344,-3.25695239730331,1.19449728689758));
#32221=CARTESIAN_POINT('Ctrl Pts',(-2.17513364606662,-2.60985014442166,
1.03799708837789));
#32222=CARTESIAN_POINT('Ctrl Pts',(-3.37785248217816,0.364021890844269,
0.881496889858204));
#32223=CARTESIAN_POINT('Ctrl Pts',(-1.56928400548455,3.01308330159882,0.724996691338513));
#32224=CARTESIAN_POINT('Ctrl Pts',(1.63823165422791,2.9766203728191,0.568496492818826));
#32225=CARTESIAN_POINT('Ctrl Pts',(3.38536312826686,0.285491005199331,0.411996294299136));
#32226=CARTESIAN_POINT('Ctrl Pts',(2.11441407237884,-2.65806374219999,0.255496095779446));
#32227=CARTESIAN_POINT('Ctrl Pts',(-1.04125416627134,-3.2360534295344,0.0989958972597585));
#32228=CARTESIAN_POINT('Ctrl Pts',(-3.26920395988323,-0.921111002274222,
-0.0575043012599318));
#32229=CARTESIAN_POINT('Ctrl Pts',(-2.81038273194434,1.15733655143344,-0.161837766939724));
#32230=CARTESIAN_POINT('Ctrl Pts',(-2.19519710401911,1.87686343907876,-0.214004499779621));
#32231=CARTESIAN_POINT('Ctrl Pts',(-0.698066426161043,-2.61113218593861,
5.21400449977962));
#32232=CARTESIAN_POINT('Ctrl Pts',(-1.55392570710631,-2.38232468520633,
5.16183776693972));
#32233=CARTESIAN_POINT('Ctrl Pts',(-3.00954808390491,-1.02260350364586,
5.05750430125993));
#32234=CARTESIAN_POINT('Ctrl Pts',(-2.51844476059198,1.94374567632669,4.90100410274025));
#32235=CARTESIAN_POINT('Ctrl Pts',(0.221656157127689,3.17078650737663,4.74450390422055));
#32236=CARTESIAN_POINT('Ctrl Pts',(2.76219456741083,1.57438115150745,4.58800370570087));
#32237=CARTESIAN_POINT('Ctrl Pts',(2.84132173890023,-1.42721226717154,4.43150350718117));
#32238=CARTESIAN_POINT('Ctrl Pts',(0.386952125103784,-3.15561484263544,
4.27500330866149));
#32239=CARTESIAN_POINT('Ctrl Pts',(-2.41209995992838,-2.07131676760884,
4.11850311014179));
#32240=CARTESIAN_POINT('Ctrl Pts',(-3.06096864280872,0.859743948080353,
3.96200291162211));
#32241=CARTESIAN_POINT('Ctrl Pts',(-0.98098504769201,3.02424170252148,3.80550271310242));
#32242=CARTESIAN_POINT('Ctrl Pts',(1.9734832757777,2.49276713404493,3.64900251458273));
#32243=CARTESIAN_POINT('Ctrl Pts',(3.16866070524613,-0.260980617462761,
3.49250231606304));
#32244=CARTESIAN_POINT('Ctrl Pts',(1.53904535272775,-2.78205328915123,3.33600211754335));
#32245=CARTESIAN_POINT('Ctrl Pts',(-1.46258511312328,-2.82300370678147,
3.17950191902366));
#32246=CARTESIAN_POINT('Ctrl Pts',(-3.16036021999547,-0.347311873155402,
3.02300172050397));
#32247=CARTESIAN_POINT('Ctrl Pts',(-2.04075132572976,2.43799745358745,2.86650152198428));
#32248=CARTESIAN_POINT('Ctrl Pts',(0.898135822920388,3.04989388087481,2.7100013234646));
#32249=CARTESIAN_POINT('Ctrl Pts',(3.03635762835191,0.942885342463967,2.5535011249449));
#32250=CARTESIAN_POINT('Ctrl Pts',(2.46774196530881,-2.00468207795258,2.39700092642522));
#32251=CARTESIAN_POINT('Ctrl Pts',(-0.300804191152645,-3.16512470461303,
2.24050072790553));
#32252=CARTESIAN_POINT('Ctrl Pts',(-2.80119087240519,-1.50393881315642,
2.08400052938584));
#32253=CARTESIAN_POINT('Ctrl Pts',(-2.80438571253693,1.49797393734019,1.92750033086615));
#32254=CARTESIAN_POINT('Ctrl Pts',(-0.307540184039062,3.16447470153125,
1.77100013234646));
#32255=CARTESIAN_POINT('Ctrl Pts',(2.46346920367124,2.00993557862573,1.61449993382677));
#32256=CARTESIAN_POINT('Ctrl Pts',(3.03835818152627,-0.936431409715195,
1.45799973530708));
#32257=CARTESIAN_POINT('Ctrl Pts',(0.904624337910361,-3.04795412470817,
1.30149953678739));
#32258=CARTESIAN_POINT('Ctrl Pts',(-2.03555556225185,-2.44237635132356,
1.1449993382677));
#32259=CARTESIAN_POINT('Ctrl Pts',(-3.16109606460172,0.340662646651362,
0.988499139748014));
#32260=CARTESIAN_POINT('Ctrl Pts',(-1.46858322563004,2.81973408171437,0.831998941228325));
#32261=CARTESIAN_POINT('Ctrl Pts',(1.53310651143252,2.78561097501341,0.675498742708636));
#32262=CARTESIAN_POINT('Ctrl Pts',(3.1681247533674,0.267171079191969,0.518998544188947));
#32263=CARTESIAN_POINT('Ctrl Pts',(1.97873235684504,-2.4874960879022,0.362498345669256));
#32264=CARTESIAN_POINT('Ctrl Pts',(-0.974437002390344,-3.02839624137338,
0.205998147149569));
#32265=CARTESIAN_POINT('Ctrl Pts',(-3.05941950588183,-0.862003411846101,
0.0494979486298786));
#32266=CARTESIAN_POINT('Ctrl Pts',(-2.63004078503903,1.08307039382515,-0.0548355170499138));
#32267=CARTESIAN_POINT('Ctrl Pts',(-2.05433155034208,1.75642532122686,-0.10700224988981));
#32268=CARTESIAN_POINT('Ctrl Pts',(-0.650199997975122,-2.43208680203507,
5.32100674966943));
#32269=CARTESIAN_POINT('Ctrl Pts',(-1.44737299166558,-2.21896863600183,
5.26884001682953));
#32270=CARTESIAN_POINT('Ctrl Pts',(-2.80318331426181,-0.952483561853041,
5.16450655114974));
#32271=CARTESIAN_POINT('Ctrl Pts',(-2.34575495521625,1.81046299814482,5.00800635263005));
#32272=CARTESIAN_POINT('Ctrl Pts',(0.206457190196319,2.95336561595388,4.85150615411036));
#32273=CARTESIAN_POINT('Ctrl Pts',(2.57279083312207,1.46642580585312,4.69500595559068));
#32274=CARTESIAN_POINT('Ctrl Pts',(2.64649225294986,-1.32934829472936,4.53850575707098));
#32275=CARTESIAN_POINT('Ctrl Pts',(0.360418810488541,-2.93923427255401,
4.3820055585513));
#32276=CARTESIAN_POINT('Ctrl Pts',(-2.24670221956701,-1.92928653725914,
4.22550536003161));
#32277=CARTESIAN_POINT('Ctrl Pts',(-2.85107796445863,0.800791289125838,
4.06900516151192));
#32278=CARTESIAN_POINT('Ctrl Pts',(-0.913718884219513,2.81686939116895,
3.91250496299223));
#32279=CARTESIAN_POINT('Ctrl Pts',(1.83816148983303,2.32183804401237,3.75600476447254));
#32280=CARTESIAN_POINT('Ctrl Pts',(2.9513855801161,-0.243085171534501,3.59950456595285));
#32281=CARTESIAN_POINT('Ctrl Pts',(1.43351298347121,-2.59128784193311,3.44300436743316));
#32282=CARTESIAN_POINT('Ctrl Pts',(-1.36229562395802,-2.62943028864365,
3.28650416891347));
#32283=CARTESIAN_POINT('Ctrl Pts',(-2.94365425929774,-0.323496691374012,
3.13000397039378));
#32284=CARTESIAN_POINT('Ctrl Pts',(-1.90081696831399,2.27082392159083,2.97350377187409));
#32285=CARTESIAN_POINT('Ctrl Pts',(0.836550632374203,2.84076259916223,2.81700357335441));
#32286=CARTESIAN_POINT('Ctrl Pts',(2.82815452773359,0.878231676507261,2.66050337483472));
#32287=CARTESIAN_POINT('Ctrl Pts',(2.29852885157487,-1.86722098954639,2.50400317631502));
#32288=CARTESIAN_POINT('Ctrl Pts',(-0.280178042015212,-2.948092043114,2.34750297779534));
#32289=CARTESIAN_POINT('Ctrl Pts',(-2.60911316073752,-1.40081369998938,
2.19100277927565));
#32290=CARTESIAN_POINT('Ctrl Pts',(-2.61208893062035,1.39525783582189,2.03450258075596));
#32291=CARTESIAN_POINT('Ctrl Pts',(-0.286452147740644,2.94748661075597,
1.87800238223627));
#32292=CARTESIAN_POINT('Ctrl Pts',(2.29454907328446,1.87211425757795,1.72150218371658));
#32293=CARTESIAN_POINT('Ctrl Pts',(2.83001790293854,-0.872220290050442,
1.56500198519689));
#32294=CARTESIAN_POINT('Ctrl Pts',(0.842594229767281,-2.83895585211302,
1.4085017866772));
#32295=CARTESIAN_POINT('Ctrl Pts',(-1.89597747843709,-2.27490255822547,
1.25200158815751));
#32296=CARTESIAN_POINT('Ctrl Pts',(-2.94433964702528,0.317303402458459,
1.09550138963782));
#32297=CARTESIAN_POINT('Ctrl Pts',(-1.36788244577553,2.6263848618299,0.939001191118136));
#32298=CARTESIAN_POINT('Ctrl Pts',(1.42798136863712,2.59460157720772,0.782500992598445));
#32299=CARTESIAN_POINT('Ctrl Pts',(2.95088637846794,0.248851153184599,0.626000794078758));
#32300=CARTESIAN_POINT('Ctrl Pts',(1.84305064131124,-2.31692843360441,0.469500595559067));
#32301=CARTESIAN_POINT('Ctrl Pts',(-0.907619838509351,-2.82073905321236,
0.31300039703938));
#32302=CARTESIAN_POINT('Ctrl Pts',(-2.84963505188044,-0.802895821417979,
0.156500198519689));
#32303=CARTESIAN_POINT('Ctrl Pts',(-2.44969883813372,1.00880423621686,0.0521667328398966));
#32304=CARTESIAN_POINT('Ctrl Pts',(-1.91346599666505,1.63598720337496,0.));
#32305=CARTESIAN_POINT('Ctrl Pts',(-1.91346599666505,1.63598720337496,0.));
#32306=CARTESIAN_POINT('Ctrl Pts',(-1.97511445450674,1.57805279092849,-2.16023702375061E-17));
#32307=CARTESIAN_POINT('Ctrl Pts',(-2.03339962644492,1.51697042789119,-3.49443898869507E-17));
#32308=CARTESIAN_POINT('Ctrl Pts',(-2.08832105501608,1.45312420295415,-1.11022302462516E-16));
#32309=CARTESIAN_POINT('Ctrl Pts',(-2.1446918579957,1.38759307857242,-1.89107908253736E-16));
#32310=CARTESIAN_POINT('Ctrl Pts',(-2.19751947843796,1.31914985899599,-1.96056269520747E-15));
#32311=CARTESIAN_POINT('Ctrl Pts',(-2.2467780277058,1.24816130047737,-2.16493489801906E-15));
#32312=CARTESIAN_POINT('Ctrl Pts',(-2.29674689545117,1.17614907224947,-2.37225419030257E-15));
#32313=CARTESIAN_POINT('Ctrl Pts',(-2.34304346389473,1.10151695033136,8.04059381600243E-19));
#32314=CARTESIAN_POINT('Ctrl Pts',(-2.38560818063646,1.02460663863002,2.77555756156289E-16));
#32315=CARTESIAN_POINT('Ctrl Pts',(-2.40516403209366,0.989271113192736,
4.04706022549276E-16));
#32316=CARTESIAN_POINT('Ctrl Pts',(-2.42393166263322,0.953454191414296,
1.85001145283656E-16));
#32317=CARTESIAN_POINT('Ctrl Pts',(-2.44190263911885,0.917186731710372,
2.77555756156289E-16));
#32318=CARTESIAN_POINT('Ctrl Pts',(-2.45212691902149,0.896552980413291,
3.30213120022811E-16));
#32319=CARTESIAN_POINT('Ctrl Pts',(-2.46209330228438,0.875773373445736,
1.0101923078241E-15));
#32320=CARTESIAN_POINT('Ctrl Pts',(-2.47179997273461,0.85485342713836,9.99200722162641E-16));
#32321=CARTESIAN_POINT('Ctrl Pts',(-2.47986685205683,0.837467580657393,
9.90065994086157E-16));
#32322=CARTESIAN_POINT('Ctrl Pts',(-2.48775634234785,0.819979991507439,
-1.29538532938285E-15));
#32323=CARTESIAN_POINT('Ctrl Pts',(-2.49545506671926,0.802422482605945,
-1.22124532708767E-15));
#32324=CARTESIAN_POINT('Ctrl Pts',(-2.53207648579799,0.718904634655909,
-8.68574941246235E-16));
#32325=CARTESIAN_POINT('Ctrl Pts',(-2.56443528935485,0.633703528135737,
-2.73580965033665E-16));
#32326=CARTESIAN_POINT('Ctrl Pts',(-2.59250335927894,0.547216632073775,
-2.22044604925031E-16));
#32327=CARTESIAN_POINT('Ctrl Pts',(-2.62102926303655,0.45931900035097,-1.696676067042E-16));
#32328=CARTESIAN_POINT('Ctrl Pts',(-2.64512381235207,0.370092536921413,
8.62583150244892E-16));
#32329=CARTESIAN_POINT('Ctrl Pts',(-2.6647184895653,0.279917395525893,9.71445146547012E-16));
#32330=CARTESIAN_POINT('Ctrl Pts',(-2.68327611608723,0.194514784532604,
1.07454560836236E-15));
#32331=CARTESIAN_POINT('Ctrl Pts',(-2.69779757345701,0.108260330337431,
1.58880599429527E-15));
#32332=CARTESIAN_POINT('Ctrl Pts',(-2.70818717658801,0.0214567600039818,
1.52655665885959E-15));
#32333=CARTESIAN_POINT('Ctrl Pts',(-2.71280574576047,-0.0171306902524466,
1.49888448909292E-15));
#32334=CARTESIAN_POINT('Ctrl Pts',(-2.71660729247955,-0.0558268492504973,
1.27797020542778E-15));
#32335=CARTESIAN_POINT('Ctrl Pts',(-2.71958083700161,-0.0946058150986653,
1.2490009027033E-15));
#32336=CARTESIAN_POINT('Ctrl Pts',(-2.72114459889708,-0.114999345005228,
1.23376619160252E-15));
#32337=CARTESIAN_POINT('Ctrl Pts',(-2.72247933944975,-0.135415780987334,
2.7744501595987E-15));
#32338=CARTESIAN_POINT('Ctrl Pts',(-2.72358327406089,-0.155851378047186,
2.83106871279415E-15));
#32339=CARTESIAN_POINT('Ctrl Pts',(-2.72441031908349,-0.171161305520925,
2.87348616409501E-15));
#32340=CARTESIAN_POINT('Ctrl Pts',(-2.72510778883702,-0.186483394270956,
-3.27116286657501E-16));
#32341=CARTESIAN_POINT('Ctrl Pts',(-2.72567444563692,-0.201797722043239,
-3.05311331771918E-16));
#32342=CARTESIAN_POINT('Ctrl Pts',(-2.72919865876058,-0.297042242048632,
-1.69699603154258E-16));
#32343=CARTESIAN_POINT('Ctrl Pts',(-2.7276765940473,-0.392142984842673,
1.65684655347014E-15));
#32344=CARTESIAN_POINT('Ctrl Pts',(-2.72104535728848,-0.486701680153984,
1.80411241501588E-15));
#32345=CARTESIAN_POINT('Ctrl Pts',(-2.71460882823241,-0.578483924102048,
1.94705422681979E-15));
#32346=CARTESIAN_POINT('Ctrl Pts',(-2.70335889560743,-0.669756429091281,
-1.44907627993903E-16));
#32347=CARTESIAN_POINT('Ctrl Pts',(-2.68719406942169,-0.760171493259568,
-2.4980018054066E-16));
#32348=CARTESIAN_POINT('Ctrl Pts',(-2.67098885106311,-0.850812483822458,
-3.27199259771174E-16));
#32349=CARTESIAN_POINT('Ctrl Pts',(-2.64984469854827,-0.940592630196976,
2.00672834831372E-15));
#32350=CARTESIAN_POINT('Ctrl Pts',(-2.62403609171522,-1.02926901742914,
1.97064586870965E-15));
#32351=CARTESIAN_POINT('Ctrl Pts',(-2.60893951244934,-1.08113970217868,
1.94953965336933E-15));
#32352=CARTESIAN_POINT('Ctrl Pts',(-2.59224593286086,-1.13263271607333,
1.51263892527377E-15));
#32353=CARTESIAN_POINT('Ctrl Pts',(-2.57400225902127,-1.18369836845093,
1.4432899320127E-15));
#32354=CARTESIAN_POINT('Ctrl Pts',(-2.56914004859136,-1.19730812434678,
1.42480739382975E-15));
#32355=CARTESIAN_POINT('Ctrl Pts',(-2.56416770379457,-1.21088751729747,
1.46101747209947E-15));
#32356=CARTESIAN_POINT('Ctrl Pts',(-2.55908604628673,-1.22443558863974,
1.41553435639707E-15));
#32357=CARTESIAN_POINT('Ctrl Pts',(-2.55396092950485,-1.23809952559165,
1.36966226068444E-15));
#32358=CARTESIAN_POINT('Ctrl Pts',(-2.54872776110117,-1.25172318692358,
7.2111001976691E-16));
#32359=CARTESIAN_POINT('Ctrl Pts',(-2.54338900633193,-1.26530267978209,
8.04911692853238E-16));
#32360=CARTESIAN_POINT('Ctrl Pts',(-2.50747702892334,-1.35664728387668,
1.36861688643376E-15));
#32361=CARTESIAN_POINT('Ctrl Pts',(-2.46677626545746,-1.44603683426546,
3.98698161417476E-15));
#32362=CARTESIAN_POINT('Ctrl Pts',(-2.42166042457756,-1.53319586749654,
3.8441472227646E-15));
#32363=CARTESIAN_POINT('Ctrl Pts',(-2.37699119409271,-1.6194920966769,3.70272677649499E-15));
#32364=CARTESIAN_POINT('Ctrl Pts',(-2.32799328414659,-1.70360251853944,
2.71566994649136E-15));
#32365=CARTESIAN_POINT('Ctrl Pts',(-2.27497251664925,-1.78525603476489,
3.10862446895044E-15));
#32366=CARTESIAN_POINT('Ctrl Pts',(-2.22143358365231,-1.86770754085407,
3.50541928807182E-15));
#32367=CARTESIAN_POINT('Ctrl Pts',(-2.16379236200239,-1.94765471708648,
2.12393071997628E-15));
#32368=CARTESIAN_POINT('Ctrl Pts',(-2.10231265300888,-2.02480256688325,
2.24820162486594E-15));
#32369=CARTESIAN_POINT('Ctrl Pts',(-2.07897144804811,-2.05409229196278,
2.29538195003625E-15));
#32370=CARTESIAN_POINT('Ctrl Pts',(-2.05507647736,-2.082978295804,3.52826900319682E-15));
#32371=CARTESIAN_POINT('Ctrl Pts',(-2.03064047373774,-2.11144345226609,
3.52495810318487E-15));
#32372=CARTESIAN_POINT('Ctrl Pts',(-2.01356997979656,-2.13132863023677,
3.52264517593754E-15));
#32373=CARTESIAN_POINT('Ctrl Pts',(-1.99623543552702,-2.15100841685411,
2.17794287054721E-15));
#32374=CARTESIAN_POINT('Ctrl Pts',(-1.97864093508987,-2.17047677606985,
2.02615701994091E-15));
#32375=CARTESIAN_POINT('Ctrl Pts',(-1.96848450504363,-2.18171489159328,
1.93853859740034E-15));
#32376=CARTESIAN_POINT('Ctrl Pts',(-1.95824406587573,-2.19287959838895,
2.78311917693584E-15));
#32377=CARTESIAN_POINT('Ctrl Pts',(-1.94792607632517,-2.20396401413293,
2.80331313717852E-15));
#32378=CARTESIAN_POINT('Ctrl Pts',(-1.87693852294064,-2.28022456377845,
2.94224716340022E-15));
#32379=CARTESIAN_POINT('Ctrl Pts',(-1.80220903731176,-2.35277040780027,
3.04985240962845E-15));
#32380=CARTESIAN_POINT('Ctrl Pts',(-1.72407227353766,-2.42127570338811,
3.40005801291454E-15));
#32381=CARTESIAN_POINT('Ctrl Pts',(-1.66546970070708,-2.472654675079,3.66271221537911E-15));
#32382=CARTESIAN_POINT('Ctrl Pts',(-1.60494926191777,-2.52176059742133,
2.66897608121856E-15));
#32383=CARTESIAN_POINT('Ctrl Pts',(-1.54263360799992,-2.56844502586205,
2.44249065417534E-15));
#32384=CARTESIAN_POINT('Ctrl Pts',(-1.50966712749181,-2.59314221193751,
2.32267441304543E-15));
#32385=CARTESIAN_POINT('Ctrl Pts',(-1.47619797745247,-2.61716151806854,
2.66421769654117E-15));
#32386=CARTESIAN_POINT('Ctrl Pts',(-1.44224276876128,-2.64047951847467,
2.55351295663786E-15));
#32387=CARTESIAN_POINT('Ctrl Pts',(-1.42523529016054,-2.65215903417213,
2.49806318714802E-15));
#32388=CARTESIAN_POINT('Ctrl Pts',(-1.40811299715223,-2.66365763094131,
1.70970381910793E-15));
#32389=CARTESIAN_POINT('Ctrl Pts',(-1.39088331342309,-2.6749694941009,1.85962356624714E-15));
#32390=CARTESIAN_POINT('Ctrl Pts',(-1.30563836789021,-2.73093564960753,
2.60136095853466E-15));
#32391=CARTESIAN_POINT('Ctrl Pts',(-1.21772994683618,-2.78235951649428,
1.84996893450162E-15));
#32392=CARTESIAN_POINT('Ctrl Pts',(-1.12744127475458,-2.82892568298919,
1.45369827286856E-15));
#32393=CARTESIAN_POINT('Ctrl Pts',(-1.06580182053759,-2.86071608395033,
1.18316702302153E-15));
#32394=CARTESIAN_POINT('Ctrl Pts',(-1.00305209219164,-2.89024190964375,
-1.85681498777599E-15));
#32395=CARTESIAN_POINT('Ctrl Pts',(-0.939272520240859,-2.91739268538644,
-2.72698530423554E-15));
#32396=CARTESIAN_POINT('Ctrl Pts',(-0.891984018423086,-2.93752326119295,
-3.3646306259368E-15));
#32397=CARTESIAN_POINT('Ctrl Pts',(-0.844129218472895,-2.95634804455667,
-1.21993627764454E-15));
#32398=CARTESIAN_POINT('Ctrl Pts',(-0.795758164394645,-2.97388052305262,
-1.30451205393456E-15));
#32399=CARTESIAN_POINT('Ctrl Pts',(-2.51644348201823,0.00207613456667446,
4.11258330249198));
#32400=CARTESIAN_POINT('Ctrl Pts',(-2.51833412820368,0.232035413192547,
4.09805725549862));
#32401=CARTESIAN_POINT('Ctrl Pts',(-2.489317966475,0.461526809188866,4.08353120850527));
#32402=CARTESIAN_POINT('Ctrl Pts',(-2.42745549360351,0.681791335068863,
4.06900516151192));
#32403=CARTESIAN_POINT('Ctrl Pts',(-2.20529160437893,1.47281732314021,4.01683842867202));
#32404=CARTESIAN_POINT('Ctrl Pts',(-1.55950524429922,2.14484335715458,3.96467169583213));
#32405=CARTESIAN_POINT('Ctrl Pts',(-0.777965335250612,2.39835114963567,
3.91250496299223));
#32406=CARTESIAN_POINT('Ctrl Pts',(0.00357457379799905,2.65185894211676,
3.86033823015234));
#32407=CARTESIAN_POINT('Ctrl Pts',(0.920868031815514,2.48684849306456,3.80817149731244));
#32408=CARTESIAN_POINT('Ctrl Pts',(1.56505210920478,1.97685606594732,3.75600476447254));
#32409=CARTESIAN_POINT('Ctrl Pts',(2.20923618659405,1.46686363883008,3.70383803163264));
#32410=CARTESIAN_POINT('Ctrl Pts',(2.58031088335508,0.611889233647789,3.65167129879275));
#32411=CARTESIAN_POINT('Ctrl Pts',(2.51286946562811,-0.206965080676461,
3.59950456595285));
#32412=CARTESIAN_POINT('Ctrl Pts',(2.44542804790114,-1.0258193950007,3.54733783311295));
#32413=CARTESIAN_POINT('Ctrl Pts',(1.93947051568617,-1.80855361846691,3.49517110027306));
#32414=CARTESIAN_POINT('Ctrl Pts',(1.22052364834049,-2.20627780465177,3.44300436743316));
#32415=CARTESIAN_POINT('Ctrl Pts',(0.501576780994809,-2.60400199083662,
3.39083763459327));
#32416=CARTESIAN_POINT('Ctrl Pts',(-0.430359421481595,-2.61671613974014,
3.33867090175337));
#32417=CARTESIAN_POINT('Ctrl Pts',(-1.15988729527642,-2.23875094798029,
3.28650416891347));
#32418=CARTESIAN_POINT('Ctrl Pts',(-1.88941516907125,-1.86078575622044,
3.23433743607358));
#32419=CARTESIAN_POINT('Ctrl Pts',(-2.4165347141845,-1.09214122379723,3.18217070323368));
#32420=CARTESIAN_POINT('Ctrl Pts',(-2.50628827157716,-0.275432188758138,
3.13000397039378));
#32421=CARTESIAN_POINT('Ctrl Pts',(-2.51627910181976,-0.18452101416286,
3.12419708109318));
#32422=CARTESIAN_POINT('Ctrl Pts',(-2.52085061170807,-0.0930142812830837,
3.11839019179258));
#32423=CARTESIAN_POINT('Ctrl Pts',(-2.52021651143941,-0.00144364612508765,
3.11258330249198));
#32424=CARTESIAN_POINT('Ctrl Pts',(-0.793799282532885,-2.96922295374569,
5.));
#32425=CARTESIAN_POINT('Ctrl Pts',(-0.886893974343616,-2.93516849963005,
5.));
#32426=CARTESIAN_POINT('Ctrl Pts',(-0.977926652176332,-2.89635378057927,
5.));
#32427=CARTESIAN_POINT('Ctrl Pts',(-1.06668684681747,-2.85310443912188,
5.));
#32428=CARTESIAN_POINT('Ctrl Pts',(-1.15738407105809,-2.80891125955214,
5.));
#32429=CARTESIAN_POINT('Ctrl Pts',(-1.2457092143346,-2.76008717620201,5.));
#32430=CARTESIAN_POINT('Ctrl Pts',(-1.33140881802392,-2.70693414934569,
5.));
#32431=CARTESIAN_POINT('Ctrl Pts',(-1.4129353161641,-2.65636938639935,5.));
#32432=CARTESIAN_POINT('Ctrl Pts',(-1.49208596169445,-2.60188611256442,
5.));
#32433=CARTESIAN_POINT('Ctrl Pts',(-1.56861084771671,-2.54371537355153,
5.));
#32434=CARTESIAN_POINT('Ctrl Pts',(-1.63557012298619,-2.49281597691525,
5.));
#32435=CARTESIAN_POINT('Ctrl Pts',(-1.70051877227587,-2.43909270266388,
5.));
#32436=CARTESIAN_POINT('Ctrl Pts',(-1.76326584581776,-2.38268809603059,
5.));
#32437=CARTESIAN_POINT('Ctrl Pts',(-1.77895171505325,-2.36858775263627,
5.));
#32438=CARTESIAN_POINT('Ctrl Pts',(-1.79450406853106,-2.35431573679482,
5.));
#32439=CARTESIAN_POINT('Ctrl Pts',(-1.80989576842494,-2.33989703960917,
5.));
#32440=CARTESIAN_POINT('Ctrl Pts',(-1.88231927767376,-2.27205185966276,
5.));
#32441=CARTESIAN_POINT('Ctrl Pts',(-1.95127665379114,-2.20088663840561,
5.));
#32442=CARTESIAN_POINT('Ctrl Pts',(-2.0165263629502,-2.1266887335995,5.));
#32443=CARTESIAN_POINT('Ctrl Pts',(-2.08140824110774,-2.05290910329586,
5.));
#32444=CARTESIAN_POINT('Ctrl Pts',(-2.14262462446156,-1.97613009459816,
5.));
#32445=CARTESIAN_POINT('Ctrl Pts',(-2.19989444056472,-1.89660745904738,
5.));
#32446=CARTESIAN_POINT('Ctrl Pts',(-2.25380452290626,-1.82175001891108,
5.));
#32447=CARTESIAN_POINT('Ctrl Pts',(-2.30421749508371,-1.74446069179507,
5.));
#32448=CARTESIAN_POINT('Ctrl Pts',(-2.35085748563793,-1.66494010874883,
5.));
#32449=CARTESIAN_POINT('Ctrl Pts',(-2.38695950989298,-1.6033866224853,5.));
#32450=CARTESIAN_POINT('Ctrl Pts',(-2.42080014316453,-1.54049593023453,
5.));
#32451=CARTESIAN_POINT('Ctrl Pts',(-2.45223267762586,-1.47635917633043,
5.));
#32452=CARTESIAN_POINT('Ctrl Pts',(-2.45885074786154,-1.46285528460488,
5.));
#32453=CARTESIAN_POINT('Ctrl Pts',(-2.46536230022247,-1.44929534936329,
5.));
#32454=CARTESIAN_POINT('Ctrl Pts',(-2.471759088022,-1.4356951550231,5.));
#32455=CARTESIAN_POINT('Ctrl Pts',(-2.51224453952186,-1.34961913912194,
5.));
#32456=CARTESIAN_POINT('Ctrl Pts',(-2.54820623907542,-1.26179296188141,
5.));
#32457=CARTESIAN_POINT('Ctrl Pts',(-2.57938608018177,-1.17245518793809,
5.));
#32458=CARTESIAN_POINT('Ctrl Pts',(-2.61056592128812,-1.08311741399478,
5.));
#32459=CARTESIAN_POINT('Ctrl Pts',(-2.63696435690728,-0.992267333350395,
5.));
#32460=CARTESIAN_POINT('Ctrl Pts',(-2.65826858221262,-0.900133621000477,
5.));
#32461=CARTESIAN_POINT('Ctrl Pts',(-2.67972778132943,-0.807329698287973,
5.));
#32462=CARTESIAN_POINT('Ctrl Pts',(-2.69601769794397,-0.713222227763925,
5.));
#32463=CARTESIAN_POINT('Ctrl Pts',(-2.70721296581232,-0.618219427263112,
5.));
#32464=CARTESIAN_POINT('Ctrl Pts',(-2.71292220509282,-0.569770946462525,
5.));
#32465=CARTESIAN_POINT('Ctrl Pts',(-2.7173056631566,-0.521089783925043,
5.));
#32466=CARTESIAN_POINT('Ctrl Pts',(-2.7203683315583,-0.472231818984886,
5.));
#32467=CARTESIAN_POINT('Ctrl Pts',(-2.72142997921888,-0.45529562564751,
5.));
#32468=CARTESIAN_POINT('Ctrl Pts',(-2.72233289252141,-0.438338201785387,
5.));
#32469=CARTESIAN_POINT('Ctrl Pts',(-2.72307719183649,-0.421361923846564,
5.));
#32470=CARTESIAN_POINT('Ctrl Pts',(-2.72371459453401,-0.40682378692649,
5.));
#32471=CARTESIAN_POINT('Ctrl Pts',(-2.72423528082335,-0.392280207970546,
5.));
#32472=CARTESIAN_POINT('Ctrl Pts',(-2.72463965223211,-0.3777370307415,5.));
#32473=CARTESIAN_POINT('Ctrl Pts',(-2.7272340736051,-0.284428925823235,
5.));
#32474=CARTESIAN_POINT('Ctrl Pts',(-2.72504745011893,-0.191078680030525,
5.));
#32475=CARTESIAN_POINT('Ctrl Pts',(-2.71820604758435,-0.0980639080872022,
5.));
#32476=CARTESIAN_POINT('Ctrl Pts',(-2.71136148545356,-0.00500617870656192,
5.));
#32477=CARTESIAN_POINT('Ctrl Pts',(-2.69985747016539,0.0877167443723885,
5.));
#32478=CARTESIAN_POINT('Ctrl Pts',(-2.68376992914425,0.179714008003965,
5.));
#32479=CARTESIAN_POINT('Ctrl Pts',(-2.66792655922036,0.27031496919411,5.));
#32480=CARTESIAN_POINT('Ctrl Pts',(-2.64763729016321,0.360212966671102,
5.));
#32481=CARTESIAN_POINT('Ctrl Pts',(-2.62293197139578,0.449008990638608,
5.));
#32482=CARTESIAN_POINT('Ctrl Pts',(-2.61350433154693,0.482893877607947,
5.));
#32483=CARTESIAN_POINT('Ctrl Pts',(-2.60343320797911,0.516617959708256,
5.));
#32484=CARTESIAN_POINT('Ctrl Pts',(-2.5927187899484,0.55015767290499,5.));
#32485=CARTESIAN_POINT('Ctrl Pts',(-2.58640692567121,0.569915919875281,
5.));
#32486=CARTESIAN_POINT('Ctrl Pts',(-2.57987179843875,0.589610167664632,
5.));
#32487=CARTESIAN_POINT('Ctrl Pts',(-2.57311332386527,0.609235450675716,
5.));
#32488=CARTESIAN_POINT('Ctrl Pts',(-2.5676510579122,0.625096798387423,5.));
#32489=CARTESIAN_POINT('Ctrl Pts',(-2.5620452571388,0.640906120496968,5.));
#32490=CARTESIAN_POINT('Ctrl Pts',(-2.55629866051782,0.656654535691256,
5.));
#32491=CARTESIAN_POINT('Ctrl Pts',(-2.52550674415446,0.741039070660769,
5.));
#32492=CARTESIAN_POINT('Ctrl Pts',(-2.4906552842231,0.823736510163055,5.));
#32493=CARTESIAN_POINT('Ctrl Pts',(-2.45179419129016,0.9043762990239,5.));
#32494=CARTESIAN_POINT('Ctrl Pts',(-2.42326911496468,0.963568049912018,
5.));
#32495=CARTESIAN_POINT('Ctrl Pts',(-2.39258278075448,1.0216506842635,5.));
#32496=CARTESIAN_POINT('Ctrl Pts',(-2.35974220291426,1.07846524994913,5.));
#32497=CARTESIAN_POINT('Ctrl Pts',(-2.34707421607123,1.10038100837762,5.));
#32498=CARTESIAN_POINT('Ctrl Pts',(-2.3340855779016,1.12210795474778,5.));
#32499=CARTESIAN_POINT('Ctrl Pts',(-2.32077630204861,1.14363645360599,5.));
#32500=CARTESIAN_POINT('Ctrl Pts',(-2.30811708022228,1.16411345368055,5.));
#32501=CARTESIAN_POINT('Ctrl Pts',(-2.29516494832623,1.18441494534906,5.));
#32502=CARTESIAN_POINT('Ctrl Pts',(-2.28193660666336,1.2045075595742,5.));
#32503=CARTESIAN_POINT('Ctrl Pts',(-2.23464292719215,1.27634223705079,5.));
#32504=CARTESIAN_POINT('Ctrl Pts',(-2.18378817877942,1.34556692931273,5.));
#32505=CARTESIAN_POINT('Ctrl Pts',(-2.12939936247367,1.41182692759809,5.));
#32506=CARTESIAN_POINT('Ctrl Pts',(-2.09060564520546,1.45908796055058,5.));
#32507=CARTESIAN_POINT('Ctrl Pts',(-2.0500132435823,1.504840036578,5.));
#32508=CARTESIAN_POINT('Ctrl Pts',(-2.00762253952656,1.54894112815615,5.));
#32509=CARTESIAN_POINT('Ctrl Pts',(-1.9782483512311,1.57950051132536,5.));
#32510=CARTESIAN_POINT('Ctrl Pts',(-1.94801045703336,1.60926686583501,5.));
#32511=CARTESIAN_POINT('Ctrl Pts',(-1.91694926235925,1.63822229446221,5.));
#32512=CARTESIAN_POINT('Origin',(0.,0.,5.));
#32513=CARTESIAN_POINT('',(2.88675134594813,-5.,5.));
#32514=CARTESIAN_POINT('',(5.77350269189626,0.,5.));
#32515=CARTESIAN_POINT('',(2.88675134594813,-5.,5.));
#32516=CARTESIAN_POINT('',(2.88675134594813,5.,5.));
#32517=CARTESIAN_POINT('',(5.77350269189626,0.,5.));
#32518=CARTESIAN_POINT('',(-2.88675134594813,5.,5.));
#32519=CARTESIAN_POINT('',(2.88675134594813,5.,5.));
#32520=CARTESIAN_POINT('',(-5.77350269189626,1.11022302462516E-15,5.));
#32521=CARTESIAN_POINT('',(-2.88675134594813,5.,5.));
#32522=CARTESIAN_POINT('',(-2.88675134594813,-5.,5.));
#32523=CARTESIAN_POINT('',(-5.77350269189626,7.07050159149938E-16,5.));
#32524=CARTESIAN_POINT('',(-2.88675134594813,-5.,5.));
#32525=CARTESIAN_POINT('Origin',(0.,0.,2.5));
#32526=CARTESIAN_POINT('Origin',(-2.88675134594813,-5.,0.));
#32527=CARTESIAN_POINT('',(-2.88675134594813,-5.,0.));
#32528=CARTESIAN_POINT('',(2.88675134594813,-5.,0.));
#32529=CARTESIAN_POINT('',(-2.88675134594813,-5.,0.));
#32530=CARTESIAN_POINT('',(2.88675134594813,-5.,0.));
#32531=CARTESIAN_POINT('',(-2.88675134594813,-5.,0.));
#32532=CARTESIAN_POINT('Origin',(-5.77350269189626,7.07050159149938E-16,
0.));
#32533=CARTESIAN_POINT('',(-5.77350269189626,7.07050159149938E-16,0.));
#32534=CARTESIAN_POINT('',(-5.77350269189626,7.07050159149938E-16,0.));
#32535=CARTESIAN_POINT('',(-5.77350269189626,7.07050159149938E-16,0.));
#32536=CARTESIAN_POINT('Origin',(-2.88675134594813,5.,0.));
#32537=CARTESIAN_POINT('',(-2.88675134594813,5.,0.));
#32538=CARTESIAN_POINT('',(-2.88675134594813,5.,0.));
#32539=CARTESIAN_POINT('',(-2.88675134594813,5.,0.));
#32540=CARTESIAN_POINT('Origin',(2.88675134594813,5.,0.));
#32541=CARTESIAN_POINT('',(2.88675134594813,5.,0.));
#32542=CARTESIAN_POINT('',(2.88675134594813,5.,0.));
#32543=CARTESIAN_POINT('',(2.88675134594813,5.,0.));
#32544=CARTESIAN_POINT('Origin',(5.77350269189626,0.,0.));
#32545=CARTESIAN_POINT('',(5.77350269189626,0.,0.));
#32546=CARTESIAN_POINT('',(5.77350269189626,0.,0.));
#32547=CARTESIAN_POINT('',(5.77350269189626,0.,0.));
#32548=CARTESIAN_POINT('Origin',(2.88675134594813,-5.,0.));
#32549=CARTESIAN_POINT('',(2.88675134594813,-5.,0.));
#32550=CARTESIAN_POINT('Origin',(0.,0.,0.));
#32551=CARTESIAN_POINT('',(0.,0.,5.));
#32552=CARTESIAN_POINT('',(0.,0.,0.));
#32553=CARTESIAN_POINT('',(0.,0.,3.));
#32554=CARTESIAN_POINT('',(-190.,-80.,0.));
#32555=CARTESIAN_POINT('',(-190.,-80.,0.));
#32556=CARTESIAN_POINT('',(-190.,-106.,-5.));
#32557=CARTESIAN_POINT('',(-190.,-55.,-5.));
#32558=CARTESIAN_POINT('',(-205.,-95.,0.));
#32559=CARTESIAN_POINT('',(-205.,-95.,-3.));
#32560=CARTESIAN_POINT('',(-160.,-95.,-3.));
#32561=CARTESIAN_POINT('',(-160.,-95.,3.));
#32562=CARTESIAN_POINT('',(-160.,-95.,4.));
#32563=CARTESIAN_POINT('',(160.,0.,0.));
#32564=CARTESIAN_POINT('',(160.,0.,25.));
#32565=CARTESIAN_POINT('',(160.,0.,3.));
#32566=CARTESIAN_POINT('',(160.,0.,4.));
#32567=CARTESIAN_POINT('',(160.,0.,29.));
#32568=CARTESIAN_POINT('',(160.,0.,30.));
#32569=CARTESIAN_POINT('',(-190.,80.,0.));
#32570=CARTESIAN_POINT('',(-190.,54.,-5.));
#32571=CARTESIAN_POINT('',(-190.,105.,-5.));
#32572=CARTESIAN_POINT('',(-190.,80.,0.));
#32573=CARTESIAN_POINT('',(-205.,-65.,0.));
#32574=CARTESIAN_POINT('',(-205.,-65.,-3.));
#32575=CARTESIAN_POINT('',(-160.,-65.,-3.));
#32576=CARTESIAN_POINT('',(-160.,-65.,3.));
#32577=CARTESIAN_POINT('',(-160.,-65.,4.));
#32578=CARTESIAN_POINT('',(-205.,65.,0.));
#32579=CARTESIAN_POINT('',(-205.,65.,-3.));
#32580=CARTESIAN_POINT('',(-160.,65.,-3.));
#32581=CARTESIAN_POINT('',(-160.,65.,3.));
#32582=CARTESIAN_POINT('',(-160.,65.,4.));
#32583=CARTESIAN_POINT('',(-205.,95.,0.));
#32584=CARTESIAN_POINT('',(-205.,95.,-3.));
#32585=CARTESIAN_POINT('',(-160.,95.,-3.));
#32586=CARTESIAN_POINT('',(-160.,95.,3.));
#32587=CARTESIAN_POINT('',(-160.,95.,4.));
#32588=UNCERTAINTY_MEASURE_WITH_UNIT(LENGTH_MEASURE(0.01),#32628,
'DISTANCE_ACCURACY_VALUE',
'Maximum model space distance between geometric entities at asserted c
onnectivities');
#32589=UNCERTAINTY_MEASURE_WITH_UNIT(LENGTH_MEASURE(0.01),#32628,
'DISTANCE_ACCURACY_VALUE',
'Maximum model space distance between geometric entities at asserted c
onnectivities');
#32590=UNCERTAINTY_MEASURE_WITH_UNIT(LENGTH_MEASURE(0.01),#32628,
'DISTANCE_ACCURACY_VALUE',
'Maximum model space distance between geometric entities at asserted c
onnectivities');
#32591=UNCERTAINTY_MEASURE_WITH_UNIT(LENGTH_MEASURE(0.01),#32628,
'DISTANCE_ACCURACY_VALUE',
'Maximum model space distance between geometric entities at asserted c
onnectivities');
#32592=UNCERTAINTY_MEASURE_WITH_UNIT(LENGTH_MEASURE(0.01),#32628,
'DISTANCE_ACCURACY_VALUE',
'Maximum model space distance between geometric entities at asserted c
onnectivities');
#32593=UNCERTAINTY_MEASURE_WITH_UNIT(LENGTH_MEASURE(0.01),#32628,
'DISTANCE_ACCURACY_VALUE',
'Maximum model space distance between geometric entities at asserted c
onnectivities');
#32594=UNCERTAINTY_MEASURE_WITH_UNIT(LENGTH_MEASURE(0.01),#32628,
'DISTANCE_ACCURACY_VALUE',
'Maximum model space distance between geometric entities at asserted c
onnectivities');
#32595=UNCERTAINTY_MEASURE_WITH_UNIT(LENGTH_MEASURE(0.01),#32628,
'DISTANCE_ACCURACY_VALUE',
'Maximum model space distance between geometric entities at asserted c
onnectivities');
#32596=UNCERTAINTY_MEASURE_WITH_UNIT(LENGTH_MEASURE(0.01),#32628,
'DISTANCE_ACCURACY_VALUE',
'Maximum model space distance between geometric entities at asserted c
onnectivities');
#32597=UNCERTAINTY_MEASURE_WITH_UNIT(LENGTH_MEASURE(0.01),#32628,
'DISTANCE_ACCURACY_VALUE',
'Maximum model space distance between geometric entities at asserted c
onnectivities');
#32598=UNCERTAINTY_MEASURE_WITH_UNIT(LENGTH_MEASURE(0.01),#32628,
'DISTANCE_ACCURACY_VALUE',
'Maximum model space distance between geometric entities at asserted c
onnectivities');
#32599=UNCERTAINTY_MEASURE_WITH_UNIT(LENGTH_MEASURE(0.01),#32628,
'DISTANCE_ACCURACY_VALUE',
'Maximum model space distance between geometric entities at asserted c
onnectivities');
#32600=UNCERTAINTY_MEASURE_WITH_UNIT(LENGTH_MEASURE(0.01),#32628,
'DISTANCE_ACCURACY_VALUE',
'Maximum model space distance between geometric entities at asserted c
onnectivities');
#32601=UNCERTAINTY_MEASURE_WITH_UNIT(LENGTH_MEASURE(0.01),#32628,
'DISTANCE_ACCURACY_VALUE',
'Maximum model space distance between geometric entities at asserted c
onnectivities');
#32602=UNCERTAINTY_MEASURE_WITH_UNIT(LENGTH_MEASURE(0.01),#32628,
'DISTANCE_ACCURACY_VALUE',
'Maximum model space distance between geometric entities at asserted c
onnectivities');
#32603=UNCERTAINTY_MEASURE_WITH_UNIT(LENGTH_MEASURE(0.01),#32628,
'DISTANCE_ACCURACY_VALUE',
'Maximum model space distance between geometric entities at asserted c
onnectivities');
#32604=UNCERTAINTY_MEASURE_WITH_UNIT(LENGTH_MEASURE(0.01),#32628,
'DISTANCE_ACCURACY_VALUE',
'Maximum model space distance between geometric entities at asserted c
onnectivities');
#32605=UNCERTAINTY_MEASURE_WITH_UNIT(LENGTH_MEASURE(0.01),#32628,
'DISTANCE_ACCURACY_VALUE',
'Maximum model space distance between geometric entities at asserted c
onnectivities');
#32606=UNCERTAINTY_MEASURE_WITH_UNIT(LENGTH_MEASURE(0.01),#32628,
'DISTANCE_ACCURACY_VALUE',
'Maximum model space distance between geometric entities at asserted c
onnectivities');
#32607=UNCERTAINTY_MEASURE_WITH_UNIT(LENGTH_MEASURE(0.01),#32628,
'DISTANCE_ACCURACY_VALUE',
'Maximum model space distance between geometric entities at asserted c
onnectivities');
#32608=(
GEOMETRIC_REPRESENTATION_CONTEXT(3)
GLOBAL_UNCERTAINTY_ASSIGNED_CONTEXT((#32588))
GLOBAL_UNIT_ASSIGNED_CONTEXT((#32628,#32630,#32631))
REPRESENTATION_CONTEXT('','3D')
);
#32609=(
GEOMETRIC_REPRESENTATION_CONTEXT(3)
GLOBAL_UNCERTAINTY_ASSIGNED_CONTEXT((#32589))
GLOBAL_UNIT_ASSIGNED_CONTEXT((#32628,#32630,#32631))
REPRESENTATION_CONTEXT('','3D')
);
#32610=(
GEOMETRIC_REPRESENTATION_CONTEXT(3)
GLOBAL_UNCERTAINTY_ASSIGNED_CONTEXT((#32590))
GLOBAL_UNIT_ASSIGNED_CONTEXT((#32628,#32630,#32631))
REPRESENTATION_CONTEXT('','3D')
);
#32611=(
GEOMETRIC_REPRESENTATION_CONTEXT(3)
GLOBAL_UNCERTAINTY_ASSIGNED_CONTEXT((#32591))
GLOBAL_UNIT_ASSIGNED_CONTEXT((#32628,#32630,#32631))
REPRESENTATION_CONTEXT('','3D')
);
#32612=(
GEOMETRIC_REPRESENTATION_CONTEXT(3)
GLOBAL_UNCERTAINTY_ASSIGNED_CONTEXT((#32592))
GLOBAL_UNIT_ASSIGNED_CONTEXT((#32628,#32630,#32631))
REPRESENTATION_CONTEXT('','3D')
);
#32613=(
GEOMETRIC_REPRESENTATION_CONTEXT(3)
GLOBAL_UNCERTAINTY_ASSIGNED_CONTEXT((#32593))
GLOBAL_UNIT_ASSIGNED_CONTEXT((#32628,#32630,#32631))
REPRESENTATION_CONTEXT('','3D')
);
#32614=(
GEOMETRIC_REPRESENTATION_CONTEXT(3)
GLOBAL_UNCERTAINTY_ASSIGNED_CONTEXT((#32594))
GLOBAL_UNIT_ASSIGNED_CONTEXT((#32628,#32630,#32631))
REPRESENTATION_CONTEXT('','3D')
);
#32615=(
GEOMETRIC_REPRESENTATION_CONTEXT(3)
GLOBAL_UNCERTAINTY_ASSIGNED_CONTEXT((#32595))
GLOBAL_UNIT_ASSIGNED_CONTEXT((#32628,#32630,#32631))
REPRESENTATION_CONTEXT('','3D')
);
#32616=(
GEOMETRIC_REPRESENTATION_CONTEXT(3)
GLOBAL_UNCERTAINTY_ASSIGNED_CONTEXT((#32596))
GLOBAL_UNIT_ASSIGNED_CONTEXT((#32628,#32630,#32631))
REPRESENTATION_CONTEXT('','3D')
);
#32617=(
GEOMETRIC_REPRESENTATION_CONTEXT(3)
GLOBAL_UNCERTAINTY_ASSIGNED_CONTEXT((#32597))
GLOBAL_UNIT_ASSIGNED_CONTEXT((#32628,#32630,#32631))
REPRESENTATION_CONTEXT('','3D')
);
#32618=(
GEOMETRIC_REPRESENTATION_CONTEXT(3)
GLOBAL_UNCERTAINTY_ASSIGNED_CONTEXT((#32598))
GLOBAL_UNIT_ASSIGNED_CONTEXT((#32628,#32630,#32631))
REPRESENTATION_CONTEXT('','3D')
);
#32619=(
GEOMETRIC_REPRESENTATION_CONTEXT(3)
GLOBAL_UNCERTAINTY_ASSIGNED_CONTEXT((#32599))
GLOBAL_UNIT_ASSIGNED_CONTEXT((#32628,#32630,#32631))
REPRESENTATION_CONTEXT('','3D')
);
#32620=(
GEOMETRIC_REPRESENTATION_CONTEXT(3)
GLOBAL_UNCERTAINTY_ASSIGNED_CONTEXT((#32600))
GLOBAL_UNIT_ASSIGNED_CONTEXT((#32628,#32630,#32631))
REPRESENTATION_CONTEXT('','3D')
);
#32621=(
GEOMETRIC_REPRESENTATION_CONTEXT(3)
GLOBAL_UNCERTAINTY_ASSIGNED_CONTEXT((#32601))
GLOBAL_UNIT_ASSIGNED_CONTEXT((#32628,#32630,#32631))
REPRESENTATION_CONTEXT('','3D')
);
#32622=(
GEOMETRIC_REPRESENTATION_CONTEXT(3)
GLOBAL_UNCERTAINTY_ASSIGNED_CONTEXT((#32602))
GLOBAL_UNIT_ASSIGNED_CONTEXT((#32628,#32630,#32631))
REPRESENTATION_CONTEXT('','3D')
);
#32623=(
GEOMETRIC_REPRESENTATION_CONTEXT(3)
GLOBAL_UNCERTAINTY_ASSIGNED_CONTEXT((#32603))
GLOBAL_UNIT_ASSIGNED_CONTEXT((#32628,#32630,#32631))
REPRESENTATION_CONTEXT('','3D')
);
#32624=(
GEOMETRIC_REPRESENTATION_CONTEXT(3)
GLOBAL_UNCERTAINTY_ASSIGNED_CONTEXT((#32604))
GLOBAL_UNIT_ASSIGNED_CONTEXT((#32628,#32630,#32631))
REPRESENTATION_CONTEXT('','3D')
);
#32625=(
GEOMETRIC_REPRESENTATION_CONTEXT(3)
GLOBAL_UNCERTAINTY_ASSIGNED_CONTEXT((#32605))
GLOBAL_UNIT_ASSIGNED_CONTEXT((#32628,#32630,#32631))
REPRESENTATION_CONTEXT('','3D')
);
#32626=(
GEOMETRIC_REPRESENTATION_CONTEXT(3)
GLOBAL_UNCERTAINTY_ASSIGNED_CONTEXT((#32606))
GLOBAL_UNIT_ASSIGNED_CONTEXT((#32628,#32630,#32631))
REPRESENTATION_CONTEXT('','3D')
);
#32627=(
GEOMETRIC_REPRESENTATION_CONTEXT(3)
GLOBAL_UNCERTAINTY_ASSIGNED_CONTEXT((#32607))
GLOBAL_UNIT_ASSIGNED_CONTEXT((#32628,#32630,#32631))
REPRESENTATION_CONTEXT('','3D')
);
#32628=(
LENGTH_UNIT()
NAMED_UNIT(*)
SI_UNIT(.MILLI.,.METRE.)
);
#32629=(
LENGTH_UNIT()
NAMED_UNIT(*)
SI_UNIT($,.METRE.)
);
#32630=(
NAMED_UNIT(*)
PLANE_ANGLE_UNIT()
SI_UNIT($,.RADIAN.)
);
#32631=(
NAMED_UNIT(*)
SI_UNIT($,.STERADIAN.)
SOLID_ANGLE_UNIT()
);
#32632=SHAPE_DEFINITION_REPRESENTATION(#32651,#32707);
#32633=SHAPE_DEFINITION_REPRESENTATION(#32652,#32708);
#32634=SHAPE_DEFINITION_REPRESENTATION(#32653,#32709);
#32635=SHAPE_DEFINITION_REPRESENTATION(#32654,#32710);
#32636=SHAPE_DEFINITION_REPRESENTATION(#32655,#32711);
#32637=SHAPE_DEFINITION_REPRESENTATION(#32656,#32712);
#32638=SHAPE_DEFINITION_REPRESENTATION(#32657,#32713);
#32639=SHAPE_DEFINITION_REPRESENTATION(#32658,#32714);
#32640=SHAPE_DEFINITION_REPRESENTATION(#32659,#32715);
#32641=SHAPE_DEFINITION_REPRESENTATION(#32660,#32716);
#32642=SHAPE_DEFINITION_REPRESENTATION(#32661,#32717);
#32643=SHAPE_DEFINITION_REPRESENTATION(#32662,#32718);
#32644=SHAPE_DEFINITION_REPRESENTATION(#32663,#32719);
#32645=SHAPE_DEFINITION_REPRESENTATION(#32664,#32720);
#32646=SHAPE_DEFINITION_REPRESENTATION(#32665,#32721);
#32647=SHAPE_DEFINITION_REPRESENTATION(#32666,#32722);
#32648=SHAPE_DEFINITION_REPRESENTATION(#32667,#32723);
#32649=SHAPE_DEFINITION_REPRESENTATION(#32668,#32724);
#32650=SHAPE_DEFINITION_REPRESENTATION(#32669,#32725);
#32651=PRODUCT_DEFINITION_SHAPE('',$,#32727);
#32652=PRODUCT_DEFINITION_SHAPE('',$,#32728);
#32653=PRODUCT_DEFINITION_SHAPE('',$,#32729);
#32654=PRODUCT_DEFINITION_SHAPE('',$,#32730);
#32655=PRODUCT_DEFINITION_SHAPE('',$,#32731);
#32656=PRODUCT_DEFINITION_SHAPE('',$,#32732);
#32657=PRODUCT_DEFINITION_SHAPE('',$,#32733);
#32658=PRODUCT_DEFINITION_SHAPE('',$,#32734);
#32659=PRODUCT_DEFINITION_SHAPE('',$,#32735);
#32660=PRODUCT_DEFINITION_SHAPE('',$,#32736);
#32661=PRODUCT_DEFINITION_SHAPE('',$,#32737);
#32662=PRODUCT_DEFINITION_SHAPE('',$,#32738);
#32663=PRODUCT_DEFINITION_SHAPE('',$,#32739);
#32664=PRODUCT_DEFINITION_SHAPE('',$,#32740);
#32665=PRODUCT_DEFINITION_SHAPE('',$,#32741);
#32666=PRODUCT_DEFINITION_SHAPE('',$,#32742);
#32667=PRODUCT_DEFINITION_SHAPE('',$,#32743);
#32668=PRODUCT_DEFINITION_SHAPE('',$,#32744);
#32669=PRODUCT_DEFINITION_SHAPE('',$,#32745);
#32670=PRODUCT_DEFINITION_SHAPE($,$,#122);
#32671=PRODUCT_DEFINITION_SHAPE($,$,#123);
#32672=PRODUCT_DEFINITION_SHAPE($,$,#124);
#32673=PRODUCT_DEFINITION_SHAPE($,$,#125);
#32674=PRODUCT_DEFINITION_SHAPE($,$,#126);
#32675=PRODUCT_DEFINITION_SHAPE($,$,#127);
#32676=PRODUCT_DEFINITION_SHAPE($,$,#128);
#32677=PRODUCT_DEFINITION_SHAPE($,$,#129);
#32678=PRODUCT_DEFINITION_SHAPE($,$,#130);
#32679=PRODUCT_DEFINITION_SHAPE($,$,#131);
#32680=PRODUCT_DEFINITION_SHAPE($,$,#132);
#32681=PRODUCT_DEFINITION_SHAPE($,$,#133);
#32682=PRODUCT_DEFINITION_SHAPE($,$,#134);
#32683=PRODUCT_DEFINITION_SHAPE($,$,#135);
#32684=PRODUCT_DEFINITION_SHAPE($,$,#136);
#32685=PRODUCT_DEFINITION_SHAPE($,$,#137);
#32686=PRODUCT_DEFINITION_SHAPE($,$,#138);
#32687=PRODUCT_DEFINITION_SHAPE($,$,#139);
#32688=PRODUCT_DEFINITION_SHAPE($,$,#140);
#32689=PRODUCT_DEFINITION_SHAPE($,$,#141);
#32690=PRODUCT_DEFINITION_SHAPE($,$,#142);
#32691=PRODUCT_DEFINITION_SHAPE($,$,#143);
#32692=PRODUCT_DEFINITION_SHAPE($,$,#144);
#32693=PRODUCT_DEFINITION_SHAPE($,$,#145);
#32694=PRODUCT_DEFINITION_SHAPE($,$,#146);
#32695=PRODUCT_DEFINITION_SHAPE($,$,#147);
#32696=PRODUCT_DEFINITION_SHAPE($,$,#148);
#32697=PRODUCT_DEFINITION_SHAPE($,$,#149);
#32698=PRODUCT_DEFINITION_SHAPE($,$,#150);
#32699=PRODUCT_DEFINITION_SHAPE($,$,#151);
#32700=PRODUCT_DEFINITION_SHAPE($,$,#152);
#32701=PRODUCT_DEFINITION_SHAPE($,$,#153);
#32702=PRODUCT_DEFINITION_SHAPE($,$,#154);
#32703=PRODUCT_DEFINITION_SHAPE($,$,#155);
#32704=PRODUCT_DEFINITION_SHAPE($,$,#156);
#32705=PRODUCT_DEFINITION_SHAPE($,$,#157);
#32706=PRODUCT_DEFINITION_SHAPE($,$,#158);
#32707=SHAPE_REPRESENTATION('',(#8892,#9492,#9493,#9494,#9495,#9496,#9497,
#9498,#9499,#9500,#9501,#9502,#9503,#9504,#9505,#9506,#9507,#9508,#9509,
#9510,#9511,#9512,#9513,#9514,#9515,#9516,#9517,#9518,#9519,#9520,#9521,
#9522,#9523,#9524,#9525,#9526,#9527,#9528),#32608);
#32708=SHAPE_REPRESENTATION('',(#8893),#32609);
#32709=SHAPE_REPRESENTATION('',(#9080),#32610);
#32710=SHAPE_REPRESENTATION('',(#9102),#32611);
#32711=SHAPE_REPRESENTATION('',(#9113),#32612);
#32712=SHAPE_REPRESENTATION('',(#9183),#32613);
#32713=SHAPE_REPRESENTATION('',(#9196),#32614);
#32714=SHAPE_REPRESENTATION('',(#9205),#32615);
#32715=SHAPE_REPRESENTATION('',(#9216),#32616);
#32716=SHAPE_REPRESENTATION('',(#9225),#32617);
#32717=SHAPE_REPRESENTATION('',(#9267),#32618);
#32718=SHAPE_REPRESENTATION('',(#9294),#32619);
#32719=SHAPE_REPRESENTATION('',(#9312),#32620);
#32720=SHAPE_REPRESENTATION('',(#9323),#32621);
#32721=SHAPE_REPRESENTATION('',(#9345),#32622);
#32722=SHAPE_REPRESENTATION('',(#9354),#32623);
#32723=SHAPE_REPRESENTATION('',(#9414),#32624);
#32724=SHAPE_REPRESENTATION('',(#9458),#32625);
#32725=SHAPE_REPRESENTATION('',(#9467),#32626);
#32726=PRODUCT_DEFINITION_CONTEXT('part definition',#32785,'design');
#32727=PRODUCT_DEFINITION('MAS-652','MAS-652',#32746,#32726);
#32728=PRODUCT_DEFINITION('Mounting frame','Mounting frame',#32747,#32726);
#32729=PRODUCT_DEFINITION('Cover panel','Cover panel',#32748,#32726);
#32730=PRODUCT_DEFINITION('Perimeter gasket','Perimeter gasket',#32749,
#32726);
#32731=PRODUCT_DEFINITION('Latch spindle','Latch spindle',#32750,#32726);
#32732=PRODUCT_DEFINITION('Latch cam','Latch cam',#32751,#32726);
#32733=PRODUCT_DEFINITION('Latch thrust washer','Latch thrust washer',#32752,
#32726);
#32734=PRODUCT_DEFINITION('Latch retaining ring','Latch retaining ring',
#32753,#32726);
#32735=PRODUCT_DEFINITION('Flat washer M4','Flat washer M4',#32754,#32726);
#32736=PRODUCT_DEFINITION('Socket head cap screw M4x8',
'Socket head cap screw M4x8',#32755,#32726);
#32737=PRODUCT_DEFINITION('Frame hinge leaf','Frame hinge leaf',#32756,
#32726);
#32738=PRODUCT_DEFINITION('Hinge pin','Hinge pin',#32757,#32726);
#32739=PRODUCT_DEFINITION('Hinge retaining ring','Hinge retaining ring',
#32758,#32726);
#32740=PRODUCT_DEFINITION('Cover hinge leaf','Cover hinge leaf',#32759,
#32726);
#32741=PRODUCT_DEFINITION('Hinge spacer','Hinge spacer',#32760,#32726);
#32742=PRODUCT_DEFINITION('Socket head cap screw M6x20',
'Socket head cap screw M6x20',#32761,#32726);
#32743=PRODUCT_DEFINITION('Socket head cap screw M6x12',
'Socket head cap screw M6x12',#32762,#32726);
#32744=PRODUCT_DEFINITION('Flat washer M6','Flat washer M6',#32763,#32726);
#32745=PRODUCT_DEFINITION('Hex nut M6','Hex nut M6',#32764,#32726);
#32746=PRODUCT_DEFINITION_FORMATION('',$,#32787);
#32747=PRODUCT_DEFINITION_FORMATION('',$,#32788);
#32748=PRODUCT_DEFINITION_FORMATION('',$,#32789);
#32749=PRODUCT_DEFINITION_FORMATION('',$,#32790);
#32750=PRODUCT_DEFINITION_FORMATION('',$,#32791);
#32751=PRODUCT_DEFINITION_FORMATION('',$,#32792);
#32752=PRODUCT_DEFINITION_FORMATION('',$,#32793);
#32753=PRODUCT_DEFINITION_FORMATION('',$,#32794);
#32754=PRODUCT_DEFINITION_FORMATION('',$,#32795);
#32755=PRODUCT_DEFINITION_FORMATION('',$,#32796);
#32756=PRODUCT_DEFINITION_FORMATION('',$,#32797);
#32757=PRODUCT_DEFINITION_FORMATION('',$,#32798);
#32758=PRODUCT_DEFINITION_FORMATION('',$,#32799);
#32759=PRODUCT_DEFINITION_FORMATION('',$,#32800);
#32760=PRODUCT_DEFINITION_FORMATION('',$,#32801);
#32761=PRODUCT_DEFINITION_FORMATION('',$,#32802);
#32762=PRODUCT_DEFINITION_FORMATION('',$,#32803);
#32763=PRODUCT_DEFINITION_FORMATION('',$,#32804);
#32764=PRODUCT_DEFINITION_FORMATION('',$,#32805);
#32765=PRODUCT_RELATED_PRODUCT_CATEGORY('MAS-652','MAS-652',(#32787));
#32766=PRODUCT_RELATED_PRODUCT_CATEGORY('Mounting frame',
'Mounting frame',(#32788));
#32767=PRODUCT_RELATED_PRODUCT_CATEGORY('Cover panel','Cover panel',(#32789));
#32768=PRODUCT_RELATED_PRODUCT_CATEGORY('Perimeter gasket',
'Perimeter gasket',(#32790));
#32769=PRODUCT_RELATED_PRODUCT_CATEGORY('Latch spindle','Latch spindle',
(#32791));
#32770=PRODUCT_RELATED_PRODUCT_CATEGORY('Latch cam','Latch cam',(#32792));
#32771=PRODUCT_RELATED_PRODUCT_CATEGORY('Latch thrust washer',
'Latch thrust washer',(#32793));
#32772=PRODUCT_RELATED_PRODUCT_CATEGORY('Latch retaining ring',
'Latch retaining ring',(#32794));
#32773=PRODUCT_RELATED_PRODUCT_CATEGORY('Flat washer M4',
'Flat washer M4',(#32795));
#32774=PRODUCT_RELATED_PRODUCT_CATEGORY('Socket head cap screw M4x8',
'Socket head cap screw M4x8',(#32796));
#32775=PRODUCT_RELATED_PRODUCT_CATEGORY('Frame hinge leaf',
'Frame hinge leaf',(#32797));
#32776=PRODUCT_RELATED_PRODUCT_CATEGORY('Hinge pin','Hinge pin',(#32798));
#32777=PRODUCT_RELATED_PRODUCT_CATEGORY('Hinge retaining ring',
'Hinge retaining ring',(#32799));
#32778=PRODUCT_RELATED_PRODUCT_CATEGORY('Cover hinge leaf',
'Cover hinge leaf',(#32800));
#32779=PRODUCT_RELATED_PRODUCT_CATEGORY('Hinge spacer','Hinge spacer',(#32801));
#32780=PRODUCT_RELATED_PRODUCT_CATEGORY('Socket head cap screw M6x20',
'Socket head cap screw M6x20',(#32802));
#32781=PRODUCT_RELATED_PRODUCT_CATEGORY('Socket head cap screw M6x12',
'Socket head cap screw M6x12',(#32803));
#32782=PRODUCT_RELATED_PRODUCT_CATEGORY('Flat washer M6',
'Flat washer M6',(#32804));
#32783=PRODUCT_RELATED_PRODUCT_CATEGORY('Hex nut M6','Hex nut M6',(#32805));
#32784=APPLICATION_PROTOCOL_DEFINITION('international standard',
'automotive_design',2009,#32785);
#32785=APPLICATION_CONTEXT(
'Core Data for Automotive Mechanical Design Process');
#32786=PRODUCT_CONTEXT('part definition',#32785,'mechanical');
#32787=PRODUCT('MAS-652','MAS-652',
'Independent hinged machine back cover with retained hinge pins, perim
eter gasket and quarter-turn cam latch. Nominal cover 360 x 260 x 3 mm
, frame 430 x 300 x 20 mm. No guarding, structural or ingress rating a
ssigned.',(#32786));
#32788=PRODUCT('Mounting frame','Mounting frame',$,(#32786));
#32789=PRODUCT('Cover panel','Cover panel',$,(#32786));
#32790=PRODUCT('Perimeter gasket','Perimeter gasket',$,(#32786));
#32791=PRODUCT('Latch spindle','Latch spindle',$,(#32786));
#32792=PRODUCT('Latch cam','Latch cam',$,(#32786));
#32793=PRODUCT('Latch thrust washer','Latch thrust washer',$,(#32786));
#32794=PRODUCT('Latch retaining ring','Latch retaining ring',$,(#32786));
#32795=PRODUCT('Flat washer M4','Flat washer M4',$,(#32786));
#32796=PRODUCT('Socket head cap screw M4x8',
'Socket head cap screw M4x8',$,(#32786));
#32797=PRODUCT('Frame hinge leaf','Frame hinge leaf',$,(#32786));
#32798=PRODUCT('Hinge pin','Hinge pin','Hinge pin',(#32786));
#32799=PRODUCT('Hinge retaining ring','Hinge retaining ring',$,(#32786));
#32800=PRODUCT('Cover hinge leaf','Cover hinge leaf',$,(#32786));
#32801=PRODUCT('Hinge spacer','Hinge spacer',$,(#32786));
#32802=PRODUCT('Socket head cap screw M6x20',
'Socket head cap screw M6x20',$,(#32786));
#32803=PRODUCT('Socket head cap screw M6x12',
'Socket head cap screw M6x12',$,(#32786));
#32804=PRODUCT('Flat washer M6','Flat washer M6',$,(#32786));
#32805=PRODUCT('Hex nut M6','Hex nut M6',$,(#32786));
#32806=PRESENTATION_STYLE_ASSIGNMENT((#32813));
#32807=PRESENTATION_STYLE_ASSIGNMENT((#32814));
#32808=PRESENTATION_STYLE_ASSIGNMENT((#32815));
#32809=PRESENTATION_STYLE_ASSIGNMENT((#32816));
#32810=PRESENTATION_STYLE_ASSIGNMENT((#32817));
#32811=PRESENTATION_STYLE_ASSIGNMENT((#32818));
#32812=PRESENTATION_STYLE_ASSIGNMENT((#32819));
#32813=SURFACE_STYLE_USAGE(.BOTH.,#32820);
#32814=SURFACE_STYLE_USAGE(.BOTH.,#32821);
#32815=SURFACE_STYLE_USAGE(.BOTH.,#32822);
#32816=SURFACE_STYLE_USAGE(.BOTH.,#32823);
#32817=SURFACE_STYLE_USAGE(.BOTH.,#32824);
#32818=SURFACE_STYLE_USAGE(.BOTH.,#32825);
#32819=SURFACE_STYLE_USAGE(.BOTH.,#32826);
#32820=SURFACE_SIDE_STYLE('',(#32827));
#32821=SURFACE_SIDE_STYLE('',(#32828));
#32822=SURFACE_SIDE_STYLE('',(#32829));
#32823=SURFACE_SIDE_STYLE('',(#32830));
#32824=SURFACE_SIDE_STYLE('',(#32831));
#32825=SURFACE_SIDE_STYLE('',(#32832));
#32826=SURFACE_SIDE_STYLE('',(#32833));
#32827=SURFACE_STYLE_FILL_AREA(#32834);
#32828=SURFACE_STYLE_FILL_AREA(#32835);
#32829=SURFACE_STYLE_FILL_AREA(#32836);
#32830=SURFACE_STYLE_FILL_AREA(#32837);
#32831=SURFACE_STYLE_FILL_AREA(#32838);
#32832=SURFACE_STYLE_FILL_AREA(#32839);
#32833=SURFACE_STYLE_FILL_AREA(#32840);
#32834=FILL_AREA_STYLE('Steel - Satin',(#32841));
#32835=FILL_AREA_STYLE('Dark blue',(#32842));
#32836=FILL_AREA_STYLE('Light blue',(#32843));
#32837=FILL_AREA_STYLE('Dark gray',(#32844));
#32838=FILL_AREA_STYLE('Gray',(#32845));
#32839=FILL_AREA_STYLE('Sky blue',(#32846));
#32840=FILL_AREA_STYLE('Light gray',(#32847));
#32841=FILL_AREA_STYLE_COLOUR('Steel - Satin',#32848);
#32842=FILL_AREA_STYLE_COLOUR('Dark blue',#32849);
#32843=FILL_AREA_STYLE_COLOUR('Light blue',#32850);
#32844=FILL_AREA_STYLE_COLOUR('Dark gray',#32851);
#32845=FILL_AREA_STYLE_COLOUR('Gray',#32852);
#32846=FILL_AREA_STYLE_COLOUR('Sky blue',#32853);
#32847=FILL_AREA_STYLE_COLOUR('Light gray',#32854);
#32848=COLOUR_RGB('Steel - Satin',0.627450980392157,0.627450980392157,0.627450980392157);
#32849=COLOUR_RGB('Dark blue',0.0901960784313725,0.270588235294118,0.513725490196078);
#32850=COLOUR_RGB('Light blue',0.662745098039216,0.831372549019608,0.949019607843137);
#32851=COLOUR_RGB('Dark gray',0.250980392156863,0.282352941176471,0.32156862745098);
#32852=COLOUR_RGB('Gray',0.407843137254902,0.447058823529412,0.498039215686275);
#32853=COLOUR_RGB('Sky blue',0.317647058823529,0.686274509803922,0.890196078431372);
#32854=COLOUR_RGB('Light gray',0.725490196078431,0.752941176470588,0.792156862745098);
ENDSEC;
END-ISO-10303-21;
